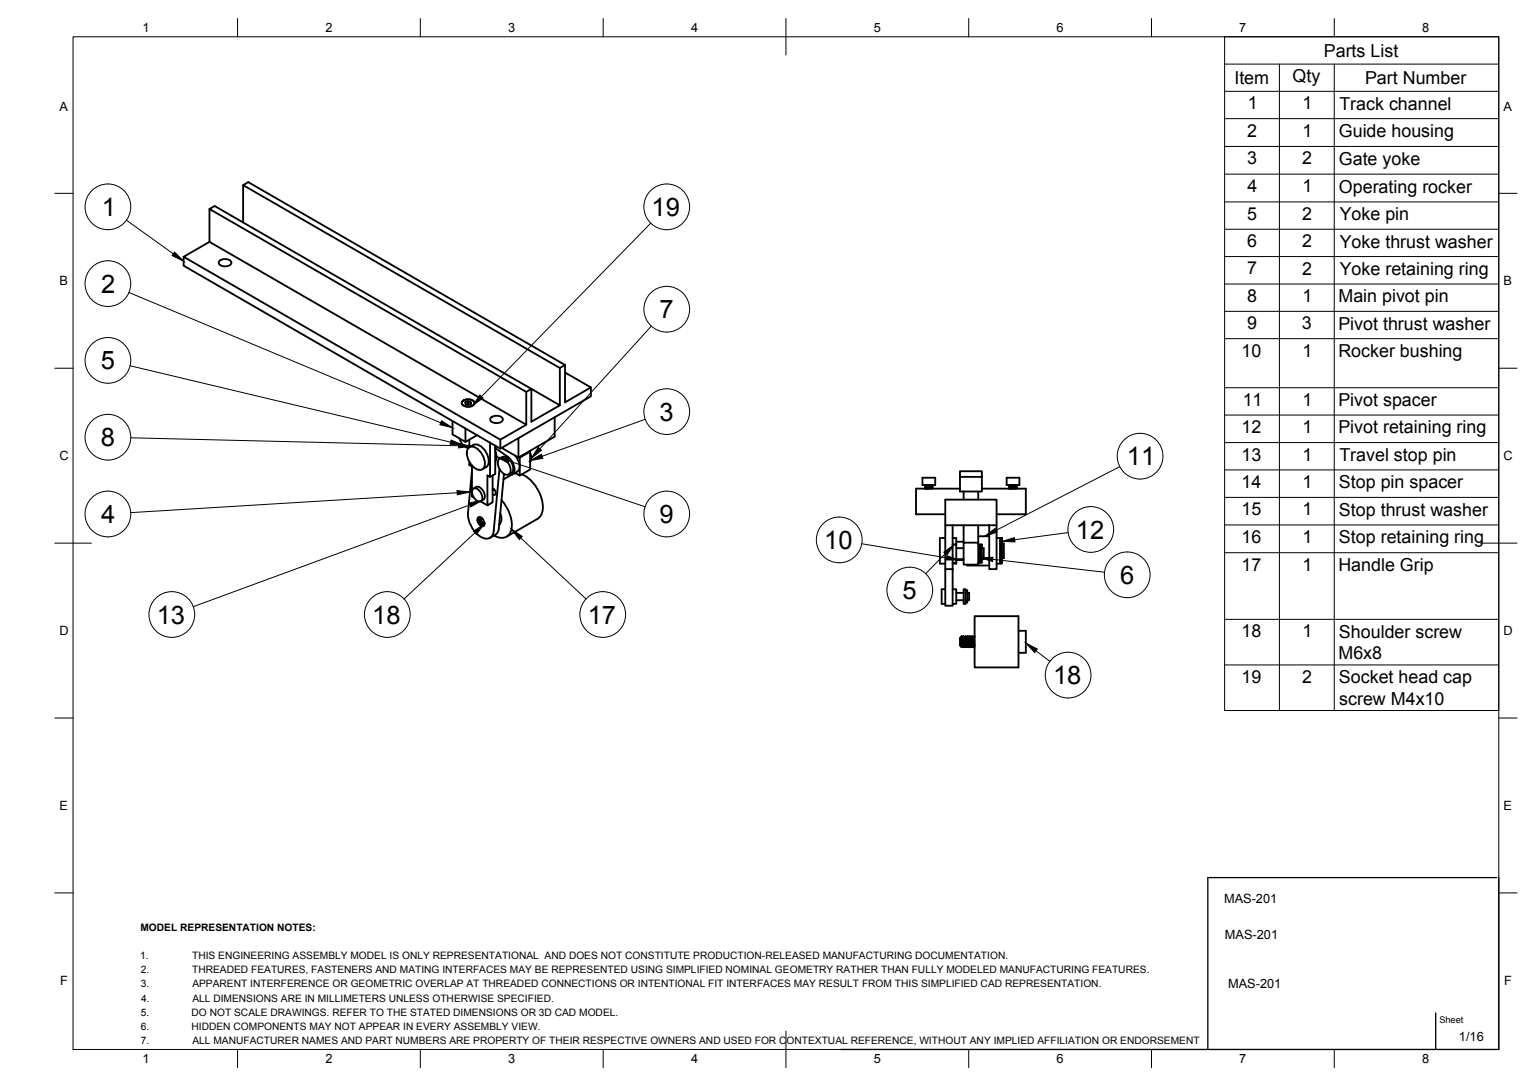
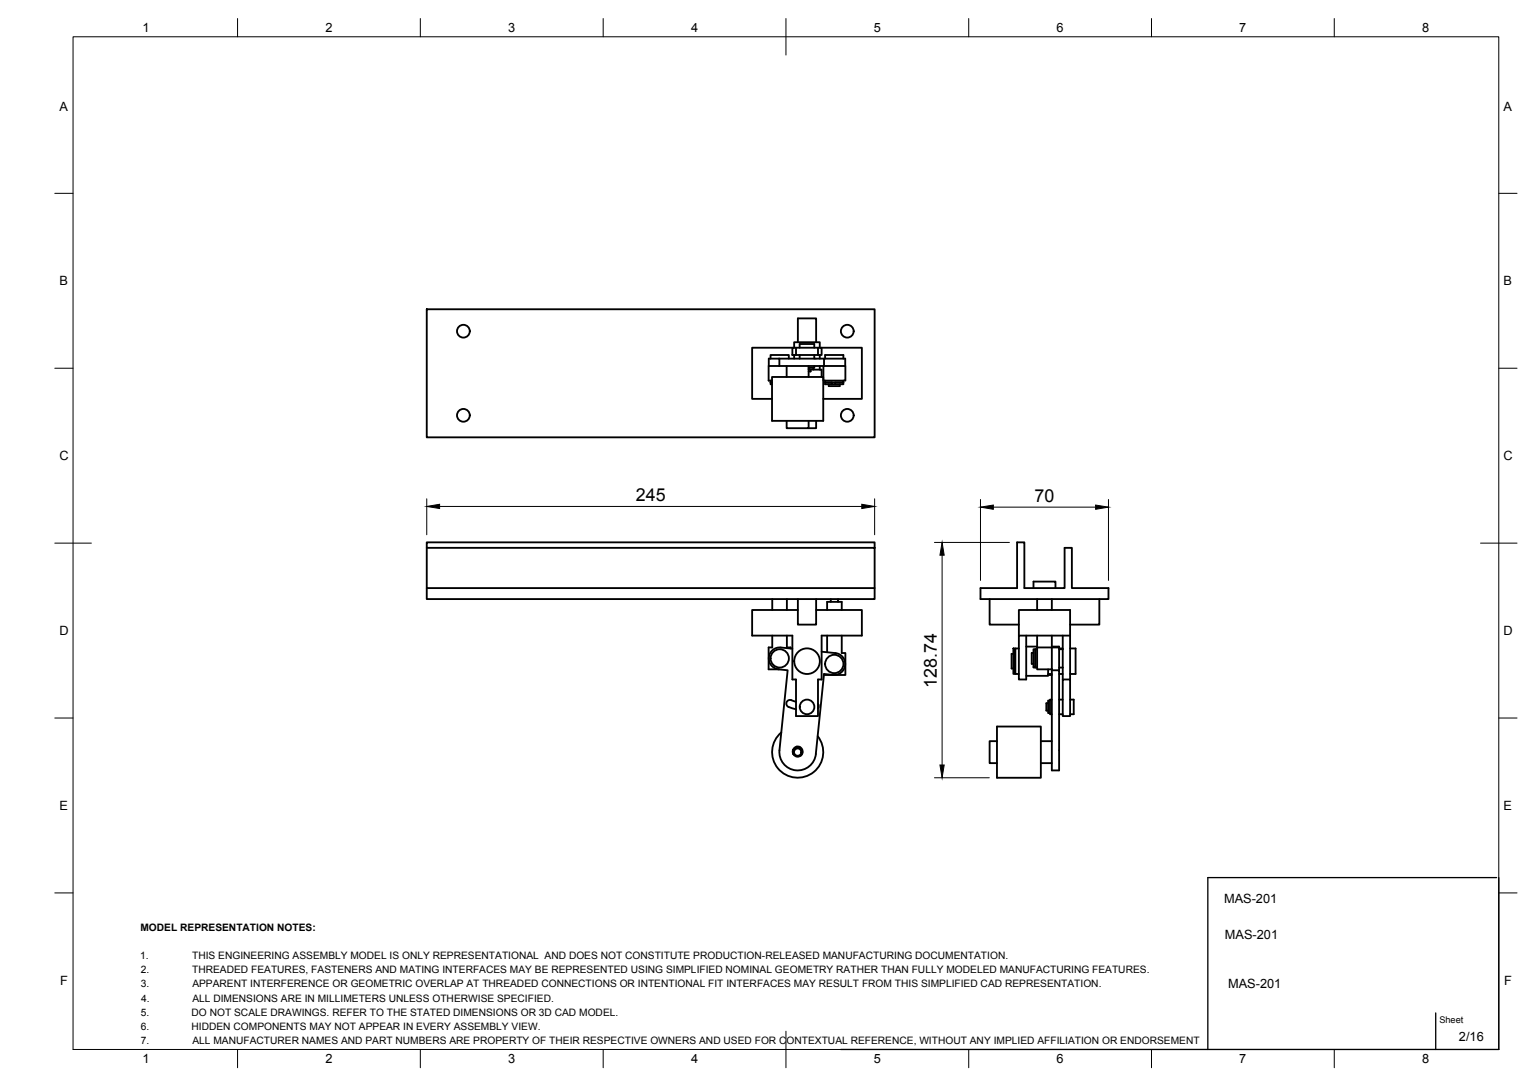
ISO-10303-21;
HEADER;
/* Generated by software containing ST-Developer
 * from STEP Tools, Inc. (www.steptools.com) 
 */

FILE_DESCRIPTION(
/* description */ ('Independent manual two-gate roller-track escapement for nominal30mm d
iameter20mm wide feed rollers. Opposed gates are driven by native capt
ured pin-slot loops with positive curved-slot travel stops at\X\B116de
g. Repeated gate/pin/washer/clip instances, adapted native common bear
ing families, full retaining lips and rotating polymer grip. External 
workpieces, gravity feeder/incline and mount anchors outside assembly.
 No powered-feed compatibility, impact, capacity, safety, force, wear 
or life rating.'),
/* implementation_level */ '2;1');

FILE_NAME(
/* name */ 'MAS-201.step',
/* time_stamp */ '2026-11-08T18:43:23-08:00',
/* author */ (''),
/* organization */ (''),
/* preprocessor_version */ 'ST-DEVELOPER v20.2',
/* originating_system */ 'Autodesk Translation Framework v15.17.0.0',
/* authorisation */ '');

FILE_SCHEMA (('AUTOMOTIVE_DESIGN { 1 0 10303 214 3 1 1 }'));
ENDSEC;

DATA;
#10=MECHANICAL_DESIGN_GEOMETRIC_PRESENTATION_REPRESENTATION('',(#455,#456,
#457,#458,#459,#460,#461,#462,#463,#464,#465,#466,#467,#468,#469,#470,#471,
#472,#473),#19863);
#11=ITEM_DEFINED_TRANSFORMATION($,$,#6654,#7165);
#12=ITEM_DEFINED_TRANSFORMATION($,$,#6703,#7166);
#13=ITEM_DEFINED_TRANSFORMATION($,$,#6899,#7167);
#14=ITEM_DEFINED_TRANSFORMATION($,$,#6827,#7168);
#15=ITEM_DEFINED_TRANSFORMATION($,$,#6926,#7169);
#16=ITEM_DEFINED_TRANSFORMATION($,$,#6962,#7170);
#17=ITEM_DEFINED_TRANSFORMATION($,$,#6899,#7171);
#18=ITEM_DEFINED_TRANSFORMATION($,$,#6926,#7172);
#19=ITEM_DEFINED_TRANSFORMATION($,$,#6971,#7173);
#20=ITEM_DEFINED_TRANSFORMATION($,$,#6944,#7174);
#21=ITEM_DEFINED_TRANSFORMATION($,$,#6991,#7175);
#22=ITEM_DEFINED_TRANSFORMATION($,$,#6962,#7176);
#23=ITEM_DEFINED_TRANSFORMATION($,$,#6971,#7177);
#24=ITEM_DEFINED_TRANSFORMATION($,$,#6982,#7178);
#25=ITEM_DEFINED_TRANSFORMATION($,$,#6991,#7179);
#26=ITEM_DEFINED_TRANSFORMATION($,$,#6991,#7180);
#27=ITEM_DEFINED_TRANSFORMATION($,$,#7000,#7181);
#28=ITEM_DEFINED_TRANSFORMATION($,$,#7009,#7182);
#29=ITEM_DEFINED_TRANSFORMATION($,$,#7020,#7183);
#30=ITEM_DEFINED_TRANSFORMATION($,$,#7038,#7184);
#31=ITEM_DEFINED_TRANSFORMATION($,$,#7047,#7185);
#32=ITEM_DEFINED_TRANSFORMATION($,$,#7056,#7186);
#33=ITEM_DEFINED_TRANSFORMATION($,$,#7067,#7187);
#34=ITEM_DEFINED_TRANSFORMATION($,$,#7076,#7188);
#35=ITEM_DEFINED_TRANSFORMATION($,$,#7117,#7189);
#36=ITEM_DEFINED_TRANSFORMATION($,$,#7117,#7190);
#37=(
REPRESENTATION_RELATIONSHIP($,$,#19935,#19934)
REPRESENTATION_RELATIONSHIP_WITH_TRANSFORMATION(#11)
SHAPE_REPRESENTATION_RELATIONSHIP()
);
#38=(
REPRESENTATION_RELATIONSHIP($,$,#19936,#19934)
REPRESENTATION_RELATIONSHIP_WITH_TRANSFORMATION(#12)
SHAPE_REPRESENTATION_RELATIONSHIP()
);
#39=(
REPRESENTATION_RELATIONSHIP($,$,#19938,#19934)
REPRESENTATION_RELATIONSHIP_WITH_TRANSFORMATION(#13)
SHAPE_REPRESENTATION_RELATIONSHIP()
);
#40=(
REPRESENTATION_RELATIONSHIP($,$,#19937,#19934)
REPRESENTATION_RELATIONSHIP_WITH_TRANSFORMATION(#14)
SHAPE_REPRESENTATION_RELATIONSHIP()
);
#41=(
REPRESENTATION_RELATIONSHIP($,$,#19939,#19934)
REPRESENTATION_RELATIONSHIP_WITH_TRANSFORMATION(#15)
SHAPE_REPRESENTATION_RELATIONSHIP()
);
#42=(
REPRESENTATION_RELATIONSHIP($,$,#19941,#19934)
REPRESENTATION_RELATIONSHIP_WITH_TRANSFORMATION(#16)
SHAPE_REPRESENTATION_RELATIONSHIP()
);
#43=(
REPRESENTATION_RELATIONSHIP($,$,#19938,#19934)
REPRESENTATION_RELATIONSHIP_WITH_TRANSFORMATION(#17)
SHAPE_REPRESENTATION_RELATIONSHIP()
);
#44=(
REPRESENTATION_RELATIONSHIP($,$,#19939,#19934)
REPRESENTATION_RELATIONSHIP_WITH_TRANSFORMATION(#18)
SHAPE_REPRESENTATION_RELATIONSHIP()
);
#45=(
REPRESENTATION_RELATIONSHIP($,$,#19942,#19934)
REPRESENTATION_RELATIONSHIP_WITH_TRANSFORMATION(#19)
SHAPE_REPRESENTATION_RELATIONSHIP()
);
#46=(
REPRESENTATION_RELATIONSHIP($,$,#19940,#19934)
REPRESENTATION_RELATIONSHIP_WITH_TRANSFORMATION(#20)
SHAPE_REPRESENTATION_RELATIONSHIP()
);
#47=(
REPRESENTATION_RELATIONSHIP($,$,#19944,#19934)
REPRESENTATION_RELATIONSHIP_WITH_TRANSFORMATION(#21)
SHAPE_REPRESENTATION_RELATIONSHIP()
);
#48=(
REPRESENTATION_RELATIONSHIP($,$,#19941,#19934)
REPRESENTATION_RELATIONSHIP_WITH_TRANSFORMATION(#22)
SHAPE_REPRESENTATION_RELATIONSHIP()
);
#49=(
REPRESENTATION_RELATIONSHIP($,$,#19942,#19934)
REPRESENTATION_RELATIONSHIP_WITH_TRANSFORMATION(#23)
SHAPE_REPRESENTATION_RELATIONSHIP()
);
#50=(
REPRESENTATION_RELATIONSHIP($,$,#19943,#19934)
REPRESENTATION_RELATIONSHIP_WITH_TRANSFORMATION(#24)
SHAPE_REPRESENTATION_RELATIONSHIP()
);
#51=(
REPRESENTATION_RELATIONSHIP($,$,#19944,#19934)
REPRESENTATION_RELATIONSHIP_WITH_TRANSFORMATION(#25)
SHAPE_REPRESENTATION_RELATIONSHIP()
);
#52=(
REPRESENTATION_RELATIONSHIP($,$,#19944,#19934)
REPRESENTATION_RELATIONSHIP_WITH_TRANSFORMATION(#26)
SHAPE_REPRESENTATION_RELATIONSHIP()
);
#53=(
REPRESENTATION_RELATIONSHIP($,$,#19945,#19934)
REPRESENTATION_RELATIONSHIP_WITH_TRANSFORMATION(#27)
SHAPE_REPRESENTATION_RELATIONSHIP()
);
#54=(
REPRESENTATION_RELATIONSHIP($,$,#19946,#19934)
REPRESENTATION_RELATIONSHIP_WITH_TRANSFORMATION(#28)
SHAPE_REPRESENTATION_RELATIONSHIP()
);
#55=(
REPRESENTATION_RELATIONSHIP($,$,#19947,#19934)
REPRESENTATION_RELATIONSHIP_WITH_TRANSFORMATION(#29)
SHAPE_REPRESENTATION_RELATIONSHIP()
);
#56=(
REPRESENTATION_RELATIONSHIP($,$,#19948,#19934)
REPRESENTATION_RELATIONSHIP_WITH_TRANSFORMATION(#30)
SHAPE_REPRESENTATION_RELATIONSHIP()
);
#57=(
REPRESENTATION_RELATIONSHIP($,$,#19949,#19934)
REPRESENTATION_RELATIONSHIP_WITH_TRANSFORMATION(#31)
SHAPE_REPRESENTATION_RELATIONSHIP()
);
#58=(
REPRESENTATION_RELATIONSHIP($,$,#19950,#19934)
REPRESENTATION_RELATIONSHIP_WITH_TRANSFORMATION(#32)
SHAPE_REPRESENTATION_RELATIONSHIP()
);
#59=(
REPRESENTATION_RELATIONSHIP($,$,#19951,#19934)
REPRESENTATION_RELATIONSHIP_WITH_TRANSFORMATION(#33)
SHAPE_REPRESENTATION_RELATIONSHIP()
);
#60=(
REPRESENTATION_RELATIONSHIP($,$,#19952,#19934)
REPRESENTATION_RELATIONSHIP_WITH_TRANSFORMATION(#34)
SHAPE_REPRESENTATION_RELATIONSHIP()
);
#61=(
REPRESENTATION_RELATIONSHIP($,$,#19953,#19934)
REPRESENTATION_RELATIONSHIP_WITH_TRANSFORMATION(#35)
SHAPE_REPRESENTATION_RELATIONSHIP()
);
#62=(
REPRESENTATION_RELATIONSHIP($,$,#19953,#19934)
REPRESENTATION_RELATIONSHIP_WITH_TRANSFORMATION(#36)
SHAPE_REPRESENTATION_RELATIONSHIP()
);
#63=CONTEXT_DEPENDENT_SHAPE_REPRESENTATION(#37,#19908);
#64=CONTEXT_DEPENDENT_SHAPE_REPRESENTATION(#38,#19909);
#65=CONTEXT_DEPENDENT_SHAPE_REPRESENTATION(#39,#19910);
#66=CONTEXT_DEPENDENT_SHAPE_REPRESENTATION(#40,#19911);
#67=CONTEXT_DEPENDENT_SHAPE_REPRESENTATION(#41,#19912);
#68=CONTEXT_DEPENDENT_SHAPE_REPRESENTATION(#42,#19913);
#69=CONTEXT_DEPENDENT_SHAPE_REPRESENTATION(#43,#19914);
#70=CONTEXT_DEPENDENT_SHAPE_REPRESENTATION(#44,#19915);
#71=CONTEXT_DEPENDENT_SHAPE_REPRESENTATION(#45,#19916);
#72=CONTEXT_DEPENDENT_SHAPE_REPRESENTATION(#46,#19917);
#73=CONTEXT_DEPENDENT_SHAPE_REPRESENTATION(#47,#19918);
#74=CONTEXT_DEPENDENT_SHAPE_REPRESENTATION(#48,#19919);
#75=CONTEXT_DEPENDENT_SHAPE_REPRESENTATION(#49,#19920);
#76=CONTEXT_DEPENDENT_SHAPE_REPRESENTATION(#50,#19921);
#77=CONTEXT_DEPENDENT_SHAPE_REPRESENTATION(#51,#19922);
#78=CONTEXT_DEPENDENT_SHAPE_REPRESENTATION(#52,#19923);
#79=CONTEXT_DEPENDENT_SHAPE_REPRESENTATION(#53,#19924);
#80=CONTEXT_DEPENDENT_SHAPE_REPRESENTATION(#54,#19925);
#81=CONTEXT_DEPENDENT_SHAPE_REPRESENTATION(#55,#19926);
#82=CONTEXT_DEPENDENT_SHAPE_REPRESENTATION(#56,#19927);
#83=CONTEXT_DEPENDENT_SHAPE_REPRESENTATION(#57,#19928);
#84=CONTEXT_DEPENDENT_SHAPE_REPRESENTATION(#58,#19929);
#85=CONTEXT_DEPENDENT_SHAPE_REPRESENTATION(#59,#19930);
#86=CONTEXT_DEPENDENT_SHAPE_REPRESENTATION(#60,#19931);
#87=CONTEXT_DEPENDENT_SHAPE_REPRESENTATION(#61,#19932);
#88=CONTEXT_DEPENDENT_SHAPE_REPRESENTATION(#62,#19933);
#89=NEXT_ASSEMBLY_USAGE_OCCURRENCE('Track channel:1','Track channel:1',
'Track channel:1',#19955,#19956,'Track channel:1');
#90=NEXT_ASSEMBLY_USAGE_OCCURRENCE('Guide housing:1','Guide housing:1',
'Guide housing:1',#19955,#19957,'Guide housing:1');
#91=NEXT_ASSEMBLY_USAGE_OCCURRENCE('Gate yoke:1','Gate yoke:1',
'Gate yoke:1',#19955,#19959,'Gate yoke:1');
#92=NEXT_ASSEMBLY_USAGE_OCCURRENCE('Operating rocker:1',
'Operating rocker:1','Operating rocker:1',#19955,#19958,
'Operating rocker:1');
#93=NEXT_ASSEMBLY_USAGE_OCCURRENCE('Yoke pin:1','Yoke pin:1',
'Yoke pin:1',#19955,#19960,'Yoke pin:1');
#94=NEXT_ASSEMBLY_USAGE_OCCURRENCE('Yoke thrust washer:1',
'Yoke thrust washer:1','Yoke thrust washer:1',#19955,#19962,
'Yoke thrust washer:1');
#95=NEXT_ASSEMBLY_USAGE_OCCURRENCE('Gate yoke:2','Gate yoke:2',
'Gate yoke:2',#19955,#19959,'Gate yoke:2');
#96=NEXT_ASSEMBLY_USAGE_OCCURRENCE('Yoke pin:2','Yoke pin:2',
'Yoke pin:2',#19955,#19960,'Yoke pin:2');
#97=NEXT_ASSEMBLY_USAGE_OCCURRENCE('Yoke retaining ring:1',
'Yoke retaining ring:1','Yoke retaining ring:1',#19955,#19963,
'Yoke retaining ring:1');
#98=NEXT_ASSEMBLY_USAGE_OCCURRENCE('Main pivot pin:1',
'Main pivot pin:1','Main pivot pin:1',#19955,#19961,'Main pivot pin:1');
#99=NEXT_ASSEMBLY_USAGE_OCCURRENCE('Pivot thrust washer:1',
'Pivot thrust washer:1','Pivot thrust washer:1',#19955,#19965,
'Pivot thrust washer:1');
#100=NEXT_ASSEMBLY_USAGE_OCCURRENCE('Yoke thrust washer:2',
'Yoke thrust washer:2','Yoke thrust washer:2',#19955,#19962,
'Yoke thrust washer:2');
#101=NEXT_ASSEMBLY_USAGE_OCCURRENCE('Yoke retaining ring:2',
'Yoke retaining ring:2','Yoke retaining ring:2',#19955,#19963,
'Yoke retaining ring:2');
#102=NEXT_ASSEMBLY_USAGE_OCCURRENCE('Rocker bushing:1',
'Rocker bushing:1','Rocker bushing:1',#19955,#19964,'Rocker bushing:1');
#103=NEXT_ASSEMBLY_USAGE_OCCURRENCE('Pivot thrust washer:2',
'Pivot thrust washer:2','Pivot thrust washer:2',#19955,#19965,
'Pivot thrust washer:2');
#104=NEXT_ASSEMBLY_USAGE_OCCURRENCE('Pivot thrust washer:3',
'Pivot thrust washer:3','Pivot thrust washer:3',#19955,#19965,
'Pivot thrust washer:3');
#105=NEXT_ASSEMBLY_USAGE_OCCURRENCE('Pivot spacer:1','Pivot spacer:1',
'Pivot spacer:1',#19955,#19966,'Pivot spacer:1');
#106=NEXT_ASSEMBLY_USAGE_OCCURRENCE('Pivot retaining ring:1',
'Pivot retaining ring:1','Pivot retaining ring:1',#19955,#19967,
'Pivot retaining ring:1');
#107=NEXT_ASSEMBLY_USAGE_OCCURRENCE('Travel stop pin:1',
'Travel stop pin:1','Travel stop pin:1',#19955,#19968,
'Travel stop pin:1');
#108=NEXT_ASSEMBLY_USAGE_OCCURRENCE('Stop pin spacer:1',
'Stop pin spacer:1','Stop pin spacer:1',#19955,#19969,
'Stop pin spacer:1');
#109=NEXT_ASSEMBLY_USAGE_OCCURRENCE('Stop thrust washer:1',
'Stop thrust washer:1','Stop thrust washer:1',#19955,#19970,
'Stop thrust washer:1');
#110=NEXT_ASSEMBLY_USAGE_OCCURRENCE('Stop retaining ring:1',
'Stop retaining ring:1','Stop retaining ring:1',#19955,#19971,
'Stop retaining ring:1');
#111=NEXT_ASSEMBLY_USAGE_OCCURRENCE('Handle grip:1','Handle grip:1',
'Handle grip:1',#19955,#19972,'Handle grip:1');
#112=NEXT_ASSEMBLY_USAGE_OCCURRENCE('Shoulder screw M6x8:1',
'Shoulder screw M6x8:1','Shoulder screw M6x8:1',#19955,#19973,
'Shoulder screw M6x8:1');
#113=NEXT_ASSEMBLY_USAGE_OCCURRENCE('Socket head cap screw M4x10:1',
'Socket head cap screw M4x10:1','Socket head cap screw M4x10:1',#19955,
#19974,'Socket head cap screw M4x10:1');
#114=NEXT_ASSEMBLY_USAGE_OCCURRENCE('Socket head cap screw M4x10:2',
'Socket head cap screw M4x10:2','Socket head cap screw M4x10:2',#19955,
#19974,'Socket head cap screw M4x10:2');
#115=CONICAL_SURFACE('',#7094,2.5,0.785398163397448);
#116=CONICAL_SURFACE('',#7146,1.5,0.785398163397449);
#117=B_SPLINE_SURFACE_WITH_KNOTS('',3,3,((#11345,#11346,#11347,#11348,#11349,
#11350,#11351,#11352,#11353,#11354,#11355,#11356,#11357,#11358,#11359,#11360,
#11361,#11362,#11363,#11364,#11365,#11366,#11367,#11368,#11369,#11370,#11371,
#11372,#11373,#11374,#11375,#11376,#11377,#11378,#11379,#11380,#11381,#11382,
#11383,#11384,#11385,#11386,#11387,#11388,#11389,#11390,#11391,#11392,#11393,
#11394,#11395,#11396,#11397,#11398,#11399,#11400,#11401,#11402,#11403,#11404,
#11405,#11406,#11407,#11408,#11409,#11410,#11411,#11412,#11413,#11414,#11415,
#11416,#11417,#11418,#11419,#11420,#11421,#11422,#11423,#11424,#11425,#11426,
#11427,#11428,#11429,#11430,#11431,#11432,#11433,#11434,#11435,#11436,#11437,
#11438,#11439,#11440,#11441,#11442,#11443,#11444,#11445,#11446,#11447,#11448),
(#11449,#11450,#11451,#11452,#11453,#11454,#11455,#11456,#11457,#11458,
#11459,#11460,#11461,#11462,#11463,#11464,#11465,#11466,#11467,#11468,#11469,
#11470,#11471,#11472,#11473,#11474,#11475,#11476,#11477,#11478,#11479,#11480,
#11481,#11482,#11483,#11484,#11485,#11486,#11487,#11488,#11489,#11490,#11491,
#11492,#11493,#11494,#11495,#11496,#11497,#11498,#11499,#11500,#11501,#11502,
#11503,#11504,#11505,#11506,#11507,#11508,#11509,#11510,#11511,#11512,#11513,
#11514,#11515,#11516,#11517,#11518,#11519,#11520,#11521,#11522,#11523,#11524,
#11525,#11526,#11527,#11528,#11529,#11530,#11531,#11532,#11533,#11534,#11535,
#11536,#11537,#11538,#11539,#11540,#11541,#11542,#11543,#11544,#11545,#11546,
#11547,#11548,#11549,#11550,#11551,#11552),(#11553,#11554,#11555,#11556,
#11557,#11558,#11559,#11560,#11561,#11562,#11563,#11564,#11565,#11566,#11567,
#11568,#11569,#11570,#11571,#11572,#11573,#11574,#11575,#11576,#11577,#11578,
#11579,#11580,#11581,#11582,#11583,#11584,#11585,#11586,#11587,#11588,#11589,
#11590,#11591,#11592,#11593,#11594,#11595,#11596,#11597,#11598,#11599,#11600,
#11601,#11602,#11603,#11604,#11605,#11606,#11607,#11608,#11609,#11610,#11611,
#11612,#11613,#11614,#11615,#11616,#11617,#11618,#11619,#11620,#11621,#11622,
#11623,#11624,#11625,#11626,#11627,#11628,#11629,#11630,#11631,#11632,#11633,
#11634,#11635,#11636,#11637,#11638,#11639,#11640,#11641,#11642,#11643,#11644,
#11645,#11646,#11647,#11648,#11649,#11650,#11651,#11652,#11653,#11654,#11655,
#11656),(#11657,#11658,#11659,#11660,#11661,#11662,#11663,#11664,#11665,
#11666,#11667,#11668,#11669,#11670,#11671,#11672,#11673,#11674,#11675,#11676,
#11677,#11678,#11679,#11680,#11681,#11682,#11683,#11684,#11685,#11686,#11687,
#11688,#11689,#11690,#11691,#11692,#11693,#11694,#11695,#11696,#11697,#11698,
#11699,#11700,#11701,#11702,#11703,#11704,#11705,#11706,#11707,#11708,#11709,
#11710,#11711,#11712,#11713,#11714,#11715,#11716,#11717,#11718,#11719,#11720,
#11721,#11722,#11723,#11724,#11725,#11726,#11727,#11728,#11729,#11730,#11731,
#11732,#11733,#11734,#11735,#11736,#11737,#11738,#11739,#11740,#11741,#11742,
#11743,#11744,#11745,#11746,#11747,#11748,#11749,#11750,#11751,#11752,#11753,
#11754,#11755,#11756,#11757,#11758,#11759,#11760)),.UNSPECIFIED.,.F.,.F.,
 .F.,(4,4),(4,1,1,1,1,1,1,1,1,1,1,1,1,1,1,1,1,1,1,1,1,1,1,1,1,1,1,1,1,1,
1,1,1,1,1,1,1,1,1,1,1,1,1,1,1,1,1,1,1,1,1,1,1,1,1,1,1,1,1,1,1,1,1,1,1,1,
1,1,1,1,1,1,1,1,1,1,1,1,1,1,1,1,1,1,1,1,1,1,1,1,1,1,1,1,1,1,1,1,1,1,1,4),
(0.,0.0448889834294942),(11.8615800042566,12.8591085386932,13.8566370731298,
14.8541656075664,15.851694142003,16.8492226764396,17.8467512108762,18.8442797453128,
19.8418082797494,20.839336814186,21.8368653486226,22.8343938830592,23.8319224174958,
24.8294509519324,25.826979486369,26.8245080208056,27.8220365552422,28.8195650896788,
29.8170936241154,30.814622158552,31.8121506929886,32.8096792274252,33.8072077618618,
34.8047362962984,35.802264830735,36.7997933651716,37.7973218996082,38.7948504340448,
39.7923789684814,40.789907502918,41.7874360373546,42.7849645717912,43.7824931062278,
44.7800216406644,45.777550175101,46.7750787095376,47.7726072439742,48.7701357784108,
49.7676643128474,50.765192847284,51.7627213817206,52.7602499161572,53.7577784505938,
54.7553069850304,55.752835519467,56.7503640539036,57.7478925883402,58.7454211227768,
59.7429496572134,60.74047819165,61.7380067260866,62.7355352605232,63.7330637949598,
64.7305923293964,65.728120863833,66.7256493982696,67.7231779327062,68.7207064671428,
69.7182350015794,70.715763536016,71.7132920704526,72.7108206048892,73.7083491393258,
74.7058776737624,75.703406208199,76.7009347426356,77.6984632770722,78.6959918115088,
79.6935203459454,80.691048880382,81.6885774148186,82.6861059492552,83.6836344836918,
84.6811630181284,85.678691552565,86.6762200870016,87.6737486214382,88.6712771558748,
89.6688056903114,90.666334224748,91.6638627591846,92.6613912936212,93.6589198280578,
94.6564483624944,95.653976896931,96.6515054313676,97.6490339658042,98.6465625002408,
99.6440910346774,100.641619569114,101.639148103551,102.636676637987,103.634205172424,
104.63173370686,105.629262241297,106.626790775734,107.62431931017,108.621847844607,
109.619376379043,110.61690491348,111.614433447917,112.611961982353),
 .UNSPECIFIED.);
#118=B_SPLINE_SURFACE_WITH_KNOTS('',3,3,((#11868,#11869,#11870,#11871,#11872,
#11873,#11874,#11875,#11876,#11877,#11878,#11879,#11880,#11881,#11882,#11883,
#11884,#11885,#11886,#11887,#11888,#11889,#11890,#11891,#11892,#11893,#11894,
#11895,#11896,#11897,#11898,#11899,#11900,#11901,#11902,#11903,#11904,#11905,
#11906,#11907,#11908,#11909,#11910,#11911,#11912,#11913,#11914,#11915,#11916,
#11917,#11918,#11919,#11920,#11921,#11922,#11923,#11924,#11925,#11926,#11927,
#11928,#11929,#11930,#11931,#11932,#11933,#11934,#11935,#11936,#11937,#11938,
#11939,#11940,#11941,#11942,#11943,#11944,#11945,#11946,#11947,#11948,#11949,
#11950,#11951,#11952,#11953,#11954,#11955,#11956,#11957,#11958,#11959,#11960,
#11961,#11962,#11963,#11964,#11965,#11966,#11967,#11968,#11969,#11970,#11971),
(#11972,#11973,#11974,#11975,#11976,#11977,#11978,#11979,#11980,#11981,
#11982,#11983,#11984,#11985,#11986,#11987,#11988,#11989,#11990,#11991,#11992,
#11993,#11994,#11995,#11996,#11997,#11998,#11999,#12000,#12001,#12002,#12003,
#12004,#12005,#12006,#12007,#12008,#12009,#12010,#12011,#12012,#12013,#12014,
#12015,#12016,#12017,#12018,#12019,#12020,#12021,#12022,#12023,#12024,#12025,
#12026,#12027,#12028,#12029,#12030,#12031,#12032,#12033,#12034,#12035,#12036,
#12037,#12038,#12039,#12040,#12041,#12042,#12043,#12044,#12045,#12046,#12047,
#12048,#12049,#12050,#12051,#12052,#12053,#12054,#12055,#12056,#12057,#12058,
#12059,#12060,#12061,#12062,#12063,#12064,#12065,#12066,#12067,#12068,#12069,
#12070,#12071,#12072,#12073,#12074,#12075),(#12076,#12077,#12078,#12079,
#12080,#12081,#12082,#12083,#12084,#12085,#12086,#12087,#12088,#12089,#12090,
#12091,#12092,#12093,#12094,#12095,#12096,#12097,#12098,#12099,#12100,#12101,
#12102,#12103,#12104,#12105,#12106,#12107,#12108,#12109,#12110,#12111,#12112,
#12113,#12114,#12115,#12116,#12117,#12118,#12119,#12120,#12121,#12122,#12123,
#12124,#12125,#12126,#12127,#12128,#12129,#12130,#12131,#12132,#12133,#12134,
#12135,#12136,#12137,#12138,#12139,#12140,#12141,#12142,#12143,#12144,#12145,
#12146,#12147,#12148,#12149,#12150,#12151,#12152,#12153,#12154,#12155,#12156,
#12157,#12158,#12159,#12160,#12161,#12162,#12163,#12164,#12165,#12166,#12167,
#12168,#12169,#12170,#12171,#12172,#12173,#12174,#12175,#12176,#12177,#12178,
#12179),(#12180,#12181,#12182,#12183,#12184,#12185,#12186,#12187,#12188,
#12189,#12190,#12191,#12192,#12193,#12194,#12195,#12196,#12197,#12198,#12199,
#12200,#12201,#12202,#12203,#12204,#12205,#12206,#12207,#12208,#12209,#12210,
#12211,#12212,#12213,#12214,#12215,#12216,#12217,#12218,#12219,#12220,#12221,
#12222,#12223,#12224,#12225,#12226,#12227,#12228,#12229,#12230,#12231,#12232,
#12233,#12234,#12235,#12236,#12237,#12238,#12239,#12240,#12241,#12242,#12243,
#12244,#12245,#12246,#12247,#12248,#12249,#12250,#12251,#12252,#12253,#12254,
#12255,#12256,#12257,#12258,#12259,#12260,#12261,#12262,#12263,#12264,#12265,
#12266,#12267,#12268,#12269,#12270,#12271,#12272,#12273,#12274,#12275,#12276,
#12277,#12278,#12279,#12280,#12281,#12282,#12283)),.UNSPECIFIED.,.F.,.F.,
 .F.,(4,4),(4,1,1,1,1,1,1,1,1,1,1,1,1,1,1,1,1,1,1,1,1,1,1,1,1,1,1,1,1,1,
1,1,1,1,1,1,1,1,1,1,1,1,1,1,1,1,1,1,1,1,1,1,1,1,1,1,1,1,1,1,1,1,1,1,1,1,
1,1,1,1,1,1,1,1,1,1,1,1,1,1,1,1,1,1,1,1,1,1,1,1,1,1,1,1,1,1,1,1,1,1,1,4),
(0.,0.0448889834294942),(14.3981410127769,15.3956695472135,16.3931980816501,
17.3907266160867,18.3882551505233,19.3857836849599,20.3833122193965,21.3808407538331,
22.3783692882697,23.3758978227063,24.3734263571429,25.3709548915795,26.3684834260161,
27.3660119604527,28.3635404948893,29.3610690293259,30.3585975637625,31.3561260981991,
32.3536546326357,33.3511831670723,34.3487117015089,35.3462402359455,36.3437687703821,
37.3412973048187,38.3388258392553,39.3363543736919,40.3338829081285,41.3314114425651,
42.3289399770017,43.3264685114383,44.3239970458749,45.3215255803115,46.3190541147481,
47.3165826491847,48.3141111836213,49.3116397180579,50.3091682524945,51.3066967869311,
52.3042253213677,53.3017538558043,54.2992823902409,55.2968109246775,56.294339459114,
57.2918679935507,58.2893965279873,59.2869250624238,60.2844535968605,61.281982131297,
62.2795106657336,63.2770392001703,64.2745677346068,65.2720962690434,66.26962480348,
67.2671533379167,68.2646818723532,69.2622104067898,70.2597389412264,71.257267475663,
72.2547960100996,73.2523245445362,74.2498530789728,75.2473816134094,76.244910147846,
77.2424386822826,78.2399672167192,79.2374957511558,80.2350242855924,81.232552820029,
82.2300813544656,83.2276098889022,84.2251384233388,85.2226669577754,86.220195492212,
87.2177240266486,88.2152525610852,89.2127810955218,90.2103096299584,91.207838164395,
92.2053666988316,93.2028952332682,94.2004237677048,95.1979523021414,96.195480836578,
97.1930093710146,98.1905379054512,99.1880664398878,100.185594974324,101.183123508761,
102.180652043198,103.178180577634,104.175709112071,105.173237646507,106.170766180944,
107.168294715381,108.165823249817,109.163351784254,110.16088031869,111.158408853127,
112.155937387564,113.153465922,114.150994456437,115.148522990873),
 .UNSPECIFIED.);
#119=B_SPLINE_SURFACE_WITH_KNOTS('',3,3,((#12588,#12589,#12590,#12591,#12592,
#12593,#12594,#12595,#12596,#12597,#12598,#12599,#12600,#12601,#12602,#12603,
#12604,#12605,#12606,#12607,#12608,#12609,#12610,#12611,#12612,#12613,#12614,
#12615,#12616,#12617,#12618,#12619,#12620,#12621,#12622,#12623,#12624,#12625,
#12626,#12627,#12628,#12629,#12630,#12631,#12632,#12633,#12634,#12635,#12636,
#12637,#12638,#12639,#12640,#12641,#12642,#12643,#12644,#12645,#12646,#12647,
#12648,#12649,#12650,#12651,#12652,#12653,#12654,#12655,#12656,#12657,#12658,
#12659,#12660,#12661,#12662,#12663,#12664,#12665,#12666,#12667,#12668,#12669,
#12670,#12671,#12672,#12673,#12674,#12675,#12676,#12677,#12678,#12679,#12680,
#12681,#12682,#12683,#12684,#12685,#12686,#12687,#12688,#12689,#12690,#12691),
(#12692,#12693,#12694,#12695,#12696,#12697,#12698,#12699,#12700,#12701,
#12702,#12703,#12704,#12705,#12706,#12707,#12708,#12709,#12710,#12711,#12712,
#12713,#12714,#12715,#12716,#12717,#12718,#12719,#12720,#12721,#12722,#12723,
#12724,#12725,#12726,#12727,#12728,#12729,#12730,#12731,#12732,#12733,#12734,
#12735,#12736,#12737,#12738,#12739,#12740,#12741,#12742,#12743,#12744,#12745,
#12746,#12747,#12748,#12749,#12750,#12751,#12752,#12753,#12754,#12755,#12756,
#12757,#12758,#12759,#12760,#12761,#12762,#12763,#12764,#12765,#12766,#12767,
#12768,#12769,#12770,#12771,#12772,#12773,#12774,#12775,#12776,#12777,#12778,
#12779,#12780,#12781,#12782,#12783,#12784,#12785,#12786,#12787,#12788,#12789,
#12790,#12791,#12792,#12793,#12794,#12795),(#12796,#12797,#12798,#12799,
#12800,#12801,#12802,#12803,#12804,#12805,#12806,#12807,#12808,#12809,#12810,
#12811,#12812,#12813,#12814,#12815,#12816,#12817,#12818,#12819,#12820,#12821,
#12822,#12823,#12824,#12825,#12826,#12827,#12828,#12829,#12830,#12831,#12832,
#12833,#12834,#12835,#12836,#12837,#12838,#12839,#12840,#12841,#12842,#12843,
#12844,#12845,#12846,#12847,#12848,#12849,#12850,#12851,#12852,#12853,#12854,
#12855,#12856,#12857,#12858,#12859,#12860,#12861,#12862,#12863,#12864,#12865,
#12866,#12867,#12868,#12869,#12870,#12871,#12872,#12873,#12874,#12875,#12876,
#12877,#12878,#12879,#12880,#12881,#12882,#12883,#12884,#12885,#12886,#12887,
#12888,#12889,#12890,#12891,#12892,#12893,#12894,#12895,#12896,#12897,#12898,
#12899),(#12900,#12901,#12902,#12903,#12904,#12905,#12906,#12907,#12908,
#12909,#12910,#12911,#12912,#12913,#12914,#12915,#12916,#12917,#12918,#12919,
#12920,#12921,#12922,#12923,#12924,#12925,#12926,#12927,#12928,#12929,#12930,
#12931,#12932,#12933,#12934,#12935,#12936,#12937,#12938,#12939,#12940,#12941,
#12942,#12943,#12944,#12945,#12946,#12947,#12948,#12949,#12950,#12951,#12952,
#12953,#12954,#12955,#12956,#12957,#12958,#12959,#12960,#12961,#12962,#12963,
#12964,#12965,#12966,#12967,#12968,#12969,#12970,#12971,#12972,#12973,#12974,
#12975,#12976,#12977,#12978,#12979,#12980,#12981,#12982,#12983,#12984,#12985,
#12986,#12987,#12988,#12989,#12990,#12991,#12992,#12993,#12994,#12995,#12996,
#12997,#12998,#12999,#13000,#13001,#13002,#13003)),.UNSPECIFIED.,.F.,.F.,
 .F.,(4,4),(4,1,1,1,1,1,1,1,1,1,1,1,1,1,1,1,1,1,1,1,1,1,1,1,1,1,1,1,1,1,
1,1,1,1,1,1,1,1,1,1,1,1,1,1,1,1,1,1,1,1,1,1,1,1,1,1,1,1,1,1,1,1,1,1,1,1,
1,1,1,1,1,1,1,1,1,1,1,1,1,1,1,1,1,1,1,1,1,1,1,1,1,1,1,1,1,1,1,1,1,1,1,4),
(0.,0.0448889834294942),(11.8615800042566,12.8591085386932,13.8566370731298,
14.8541656075664,15.851694142003,16.8492226764396,17.8467512108762,18.8442797453128,
19.8418082797494,20.839336814186,21.8368653486226,22.8343938830592,23.8319224174958,
24.8294509519324,25.826979486369,26.8245080208056,27.8220365552422,28.8195650896788,
29.8170936241154,30.814622158552,31.8121506929886,32.8096792274252,33.8072077618618,
34.8047362962984,35.802264830735,36.7997933651716,37.7973218996082,38.7948504340448,
39.7923789684814,40.789907502918,41.7874360373546,42.7849645717912,43.7824931062278,
44.7800216406644,45.777550175101,46.7750787095376,47.7726072439742,48.7701357784108,
49.7676643128474,50.765192847284,51.7627213817206,52.7602499161572,53.7577784505938,
54.7553069850304,55.752835519467,56.7503640539036,57.7478925883402,58.7454211227768,
59.7429496572134,60.74047819165,61.7380067260866,62.7355352605232,63.7330637949598,
64.7305923293964,65.728120863833,66.7256493982696,67.7231779327062,68.7207064671428,
69.7182350015794,70.715763536016,71.7132920704526,72.7108206048892,73.7083491393258,
74.7058776737624,75.703406208199,76.7009347426356,77.6984632770722,78.6959918115088,
79.6935203459454,80.691048880382,81.6885774148186,82.6861059492552,83.6836344836918,
84.6811630181284,85.678691552565,86.6762200870016,87.6737486214382,88.6712771558748,
89.6688056903114,90.666334224748,91.6638627591846,92.6613912936212,93.6589198280578,
94.6564483624944,95.653976896931,96.6515054313676,97.6490339658042,98.6465625002408,
99.6440910346774,100.641619569114,101.639148103551,102.636676637987,103.634205172424,
104.63173370686,105.629262241297,106.626790775734,107.62431931017,108.621847844607,
109.619376379043,110.61690491348,111.614433447917,112.611961982353),
 .UNSPECIFIED.);
#120=B_SPLINE_SURFACE_WITH_KNOTS('',3,3,((#13111,#13112,#13113,#13114,#13115,
#13116,#13117,#13118,#13119,#13120,#13121,#13122,#13123,#13124,#13125,#13126,
#13127,#13128,#13129,#13130,#13131,#13132,#13133,#13134,#13135,#13136,#13137,
#13138,#13139,#13140,#13141,#13142,#13143,#13144,#13145,#13146,#13147,#13148,
#13149,#13150,#13151,#13152,#13153,#13154,#13155,#13156,#13157,#13158,#13159,
#13160,#13161,#13162,#13163,#13164,#13165,#13166,#13167,#13168,#13169,#13170,
#13171,#13172,#13173,#13174,#13175,#13176,#13177,#13178,#13179,#13180,#13181,
#13182,#13183,#13184,#13185,#13186,#13187,#13188,#13189,#13190,#13191,#13192,
#13193,#13194,#13195,#13196,#13197,#13198,#13199,#13200,#13201,#13202,#13203,
#13204,#13205,#13206,#13207,#13208,#13209,#13210,#13211,#13212,#13213,#13214),
(#13215,#13216,#13217,#13218,#13219,#13220,#13221,#13222,#13223,#13224,
#13225,#13226,#13227,#13228,#13229,#13230,#13231,#13232,#13233,#13234,#13235,
#13236,#13237,#13238,#13239,#13240,#13241,#13242,#13243,#13244,#13245,#13246,
#13247,#13248,#13249,#13250,#13251,#13252,#13253,#13254,#13255,#13256,#13257,
#13258,#13259,#13260,#13261,#13262,#13263,#13264,#13265,#13266,#13267,#13268,
#13269,#13270,#13271,#13272,#13273,#13274,#13275,#13276,#13277,#13278,#13279,
#13280,#13281,#13282,#13283,#13284,#13285,#13286,#13287,#13288,#13289,#13290,
#13291,#13292,#13293,#13294,#13295,#13296,#13297,#13298,#13299,#13300,#13301,
#13302,#13303,#13304,#13305,#13306,#13307,#13308,#13309,#13310,#13311,#13312,
#13313,#13314,#13315,#13316,#13317,#13318),(#13319,#13320,#13321,#13322,
#13323,#13324,#13325,#13326,#13327,#13328,#13329,#13330,#13331,#13332,#13333,
#13334,#13335,#13336,#13337,#13338,#13339,#13340,#13341,#13342,#13343,#13344,
#13345,#13346,#13347,#13348,#13349,#13350,#13351,#13352,#13353,#13354,#13355,
#13356,#13357,#13358,#13359,#13360,#13361,#13362,#13363,#13364,#13365,#13366,
#13367,#13368,#13369,#13370,#13371,#13372,#13373,#13374,#13375,#13376,#13377,
#13378,#13379,#13380,#13381,#13382,#13383,#13384,#13385,#13386,#13387,#13388,
#13389,#13390,#13391,#13392,#13393,#13394,#13395,#13396,#13397,#13398,#13399,
#13400,#13401,#13402,#13403,#13404,#13405,#13406,#13407,#13408,#13409,#13410,
#13411,#13412,#13413,#13414,#13415,#13416,#13417,#13418,#13419,#13420,#13421,
#13422),(#13423,#13424,#13425,#13426,#13427,#13428,#13429,#13430,#13431,
#13432,#13433,#13434,#13435,#13436,#13437,#13438,#13439,#13440,#13441,#13442,
#13443,#13444,#13445,#13446,#13447,#13448,#13449,#13450,#13451,#13452,#13453,
#13454,#13455,#13456,#13457,#13458,#13459,#13460,#13461,#13462,#13463,#13464,
#13465,#13466,#13467,#13468,#13469,#13470,#13471,#13472,#13473,#13474,#13475,
#13476,#13477,#13478,#13479,#13480,#13481,#13482,#13483,#13484,#13485,#13486,
#13487,#13488,#13489,#13490,#13491,#13492,#13493,#13494,#13495,#13496,#13497,
#13498,#13499,#13500,#13501,#13502,#13503,#13504,#13505,#13506,#13507,#13508,
#13509,#13510,#13511,#13512,#13513,#13514,#13515,#13516,#13517,#13518,#13519,
#13520,#13521,#13522,#13523,#13524,#13525,#13526)),.UNSPECIFIED.,.F.,.F.,
 .F.,(4,4),(4,1,1,1,1,1,1,1,1,1,1,1,1,1,1,1,1,1,1,1,1,1,1,1,1,1,1,1,1,1,
1,1,1,1,1,1,1,1,1,1,1,1,1,1,1,1,1,1,1,1,1,1,1,1,1,1,1,1,1,1,1,1,1,1,1,1,
1,1,1,1,1,1,1,1,1,1,1,1,1,1,1,1,1,1,1,1,1,1,1,1,1,1,1,1,1,1,1,1,1,1,1,4),
(0.,0.0448889834294942),(14.3981410127769,15.3956695472135,16.3931980816501,
17.3907266160867,18.3882551505233,19.3857836849599,20.3833122193965,21.3808407538331,
22.3783692882697,23.3758978227063,24.3734263571429,25.3709548915795,26.3684834260161,
27.3660119604527,28.3635404948893,29.3610690293259,30.3585975637625,31.3561260981991,
32.3536546326357,33.3511831670723,34.3487117015089,35.3462402359455,36.3437687703821,
37.3412973048187,38.3388258392553,39.3363543736919,40.3338829081285,41.3314114425651,
42.3289399770017,43.3264685114383,44.3239970458749,45.3215255803115,46.3190541147481,
47.3165826491847,48.3141111836213,49.3116397180579,50.3091682524945,51.3066967869311,
52.3042253213677,53.3017538558043,54.2992823902409,55.2968109246775,56.294339459114,
57.2918679935507,58.2893965279873,59.2869250624238,60.2844535968605,61.281982131297,
62.2795106657336,63.2770392001703,64.2745677346068,65.2720962690434,66.26962480348,
67.2671533379167,68.2646818723532,69.2622104067898,70.2597389412264,71.257267475663,
72.2547960100996,73.2523245445362,74.2498530789728,75.2473816134094,76.244910147846,
77.2424386822826,78.2399672167192,79.2374957511558,80.2350242855924,81.232552820029,
82.2300813544656,83.2276098889022,84.2251384233388,85.2226669577754,86.220195492212,
87.2177240266486,88.2152525610852,89.2127810955218,90.2103096299584,91.207838164395,
92.2053666988316,93.2028952332682,94.2004237677048,95.1979523021414,96.195480836578,
97.1930093710146,98.1905379054512,99.1880664398878,100.185594974324,101.183123508761,
102.180652043198,103.178180577634,104.175709112071,105.173237646507,106.170766180944,
107.168294715381,108.165823249817,109.163351784254,110.16088031869,111.158408853127,
112.155937387564,113.153465922,114.150994456437,115.148522990873),
 .UNSPECIFIED.);
#121=B_SPLINE_SURFACE_WITH_KNOTS('',3,3,((#14592,#14593,#14594,#14595,#14596,
#14597,#14598,#14599,#14600,#14601,#14602,#14603,#14604,#14605,#14606,#14607,
#14608,#14609,#14610,#14611,#14612,#14613,#14614,#14615,#14616,#14617,#14618,
#14619,#14620,#14621,#14622,#14623,#14624,#14625,#14626,#14627,#14628,#14629,
#14630,#14631,#14632,#14633,#14634,#14635,#14636,#14637,#14638,#14639,#14640,
#14641,#14642,#14643,#14644,#14645,#14646,#14647,#14648,#14649,#14650,#14651,
#14652,#14653,#14654,#14655,#14656,#14657,#14658,#14659),(#14660,#14661,
#14662,#14663,#14664,#14665,#14666,#14667,#14668,#14669,#14670,#14671,#14672,
#14673,#14674,#14675,#14676,#14677,#14678,#14679,#14680,#14681,#14682,#14683,
#14684,#14685,#14686,#14687,#14688,#14689,#14690,#14691,#14692,#14693,#14694,
#14695,#14696,#14697,#14698,#14699,#14700,#14701,#14702,#14703,#14704,#14705,
#14706,#14707,#14708,#14709,#14710,#14711,#14712,#14713,#14714,#14715,#14716,
#14717,#14718,#14719,#14720,#14721,#14722,#14723,#14724,#14725,#14726,#14727),
(#14728,#14729,#14730,#14731,#14732,#14733,#14734,#14735,#14736,#14737,
#14738,#14739,#14740,#14741,#14742,#14743,#14744,#14745,#14746,#14747,#14748,
#14749,#14750,#14751,#14752,#14753,#14754,#14755,#14756,#14757,#14758,#14759,
#14760,#14761,#14762,#14763,#14764,#14765,#14766,#14767,#14768,#14769,#14770,
#14771,#14772,#14773,#14774,#14775,#14776,#14777,#14778,#14779,#14780,#14781,
#14782,#14783,#14784,#14785,#14786,#14787,#14788,#14789,#14790,#14791,#14792,
#14793,#14794,#14795),(#14796,#14797,#14798,#14799,#14800,#14801,#14802,
#14803,#14804,#14805,#14806,#14807,#14808,#14809,#14810,#14811,#14812,#14813,
#14814,#14815,#14816,#14817,#14818,#14819,#14820,#14821,#14822,#14823,#14824,
#14825,#14826,#14827,#14828,#14829,#14830,#14831,#14832,#14833,#14834,#14835,
#14836,#14837,#14838,#14839,#14840,#14841,#14842,#14843,#14844,#14845,#14846,
#14847,#14848,#14849,#14850,#14851,#14852,#14853,#14854,#14855,#14856,#14857,
#14858,#14859,#14860,#14861,#14862,#14863)),.UNSPECIFIED.,.F.,.F.,.F.,(4,
4),(4,1,1,1,1,1,1,1,1,1,1,1,1,1,1,1,1,1,1,1,1,1,1,1,1,1,1,1,1,1,1,1,1,1,
1,1,1,1,1,1,1,1,1,1,1,1,1,1,1,1,1,1,1,1,1,1,1,1,1,1,1,1,1,1,1,4),(0.,0.0642013499338864),
(11.8589888623078,12.8566626771512,13.8543364919947,14.8520103068381,15.8496841216816,
16.8473579365251,17.8450317513685,18.842705566212,19.8403793810554,20.8380531958989,
21.8357270107423,22.8334008255858,23.8310746404292,24.8287484552727,25.8264222701161,
26.8240960849596,27.821769899803,28.8194437146465,29.8171175294899,30.8147913443334,
31.8124651591768,32.8101389740203,33.8078127888637,34.8054866037072,35.8031604185506,
36.8008342333941,37.7985080482375,38.796181863081,39.7938556779244,40.7915294927679,
41.7892033076113,42.7868771224548,43.7845509372982,44.7822247521417,45.7798985669851,
46.7775723818286,47.775246196672,48.7729200115155,49.7705938263589,50.7682676412024,
51.7659414560458,52.7636152708893,53.7612890857327,54.7589629005762,55.7566367154196,
56.7543105302631,57.7519843451065,58.74965815995,59.7473319747934,60.7450057896369,
61.7426796044803,62.7403534193238,63.7380272341672,64.7357010490107,65.7333748638542,
66.7310486786976,67.728722493541,68.7263963083845,69.7240701232279,70.7217439380714,
71.7194177529149,72.7170915677583,73.7147653826018,74.7124391974452,75.7101130122887,
76.7077868271321),.UNSPECIFIED.);
#122=B_SPLINE_SURFACE_WITH_KNOTS('',3,3,((#15080,#15081,#15082,#15083,#15084,
#15085,#15086,#15087,#15088,#15089,#15090,#15091,#15092,#15093,#15094,#15095,
#15096,#15097,#15098,#15099,#15100,#15101,#15102,#15103,#15104,#15105,#15106,
#15107,#15108,#15109,#15110,#15111,#15112,#15113,#15114,#15115,#15116,#15117,
#15118,#15119,#15120,#15121,#15122,#15123,#15124,#15125,#15126,#15127,#15128,
#15129,#15130,#15131,#15132,#15133,#15134,#15135,#15136,#15137,#15138,#15139,
#15140,#15141,#15142,#15143,#15144,#15145,#15146,#15147),(#15148,#15149,
#15150,#15151,#15152,#15153,#15154,#15155,#15156,#15157,#15158,#15159,#15160,
#15161,#15162,#15163,#15164,#15165,#15166,#15167,#15168,#15169,#15170,#15171,
#15172,#15173,#15174,#15175,#15176,#15177,#15178,#15179,#15180,#15181,#15182,
#15183,#15184,#15185,#15186,#15187,#15188,#15189,#15190,#15191,#15192,#15193,
#15194,#15195,#15196,#15197,#15198,#15199,#15200,#15201,#15202,#15203,#15204,
#15205,#15206,#15207,#15208,#15209,#15210,#15211,#15212,#15213,#15214,#15215),
(#15216,#15217,#15218,#15219,#15220,#15221,#15222,#15223,#15224,#15225,
#15226,#15227,#15228,#15229,#15230,#15231,#15232,#15233,#15234,#15235,#15236,
#15237,#15238,#15239,#15240,#15241,#15242,#15243,#15244,#15245,#15246,#15247,
#15248,#15249,#15250,#15251,#15252,#15253,#15254,#15255,#15256,#15257,#15258,
#15259,#15260,#15261,#15262,#15263,#15264,#15265,#15266,#15267,#15268,#15269,
#15270,#15271,#15272,#15273,#15274,#15275,#15276,#15277,#15278,#15279,#15280,
#15281,#15282,#15283),(#15284,#15285,#15286,#15287,#15288,#15289,#15290,
#15291,#15292,#15293,#15294,#15295,#15296,#15297,#15298,#15299,#15300,#15301,
#15302,#15303,#15304,#15305,#15306,#15307,#15308,#15309,#15310,#15311,#15312,
#15313,#15314,#15315,#15316,#15317,#15318,#15319,#15320,#15321,#15322,#15323,
#15324,#15325,#15326,#15327,#15328,#15329,#15330,#15331,#15332,#15333,#15334,
#15335,#15336,#15337,#15338,#15339,#15340,#15341,#15342,#15343,#15344,#15345,
#15346,#15347,#15348,#15349,#15350,#15351)),.UNSPECIFIED.,.F.,.F.,.F.,(4,
4),(4,1,1,1,1,1,1,1,1,1,1,1,1,1,1,1,1,1,1,1,1,1,1,1,1,1,1,1,1,1,1,1,1,1,
1,1,1,1,1,1,1,1,1,1,1,1,1,1,1,1,1,1,1,1,1,1,1,1,1,1,1,1,1,1,1,4),(0.,0.0642013499338864),
(14.3984001269718,15.3960739418153,16.3937477566587,17.3914215715022,18.3890953863456,
19.3867692011891,20.3844430160325,21.382116830876,22.3797906457194,23.3774644605629,
24.3751382754063,25.3728120902498,26.3704859050932,27.3681597199367,28.3658335347801,
29.3635073496236,30.361181164467,31.3588549793105,32.3565287941539,33.3542026089974,
34.3518764238408,35.3495502386843,36.3472240535278,37.3448978683712,38.3425716832147,
39.3402454980581,40.3379193129016,41.335593127745,42.3332669425885,43.3309407574319,
44.3286145722754,45.3262883871188,46.3239622019623,47.3216360168057,48.3193098316492,
49.3169836464926,50.3146574613361,51.3123312761795,52.310005091023,53.3076789058664,
54.3053527207099,55.3030265355533,56.3007003503968,57.2983741652402,58.2960479800837,
59.2937217949271,60.2913956097706,61.289069424614,62.2867432394575,63.2844170543009,
64.2820908691444,65.2797646839878,66.2774384988313,67.2751123136747,68.2727861285182,
69.2704599433616,70.2681337582051,71.2658075730485,72.263481387892,73.2611552027354,
74.2588290175789,75.2565028324223,76.2541766472658,77.2518504621092,78.2495242769527,
79.2471980917962),.UNSPECIFIED.);
#123=B_SPLINE_SURFACE_WITH_KNOTS('',3,3,((#16881,#16882,#16883,#16884,#16885,
#16886,#16887,#16888,#16889,#16890,#16891,#16892,#16893,#16894,#16895,#16896,
#16897,#16898,#16899,#16900,#16901,#16902,#16903,#16904,#16905,#16906,#16907,
#16908,#16909,#16910,#16911,#16912,#16913,#16914,#16915,#16916,#16917,#16918,
#16919,#16920,#16921,#16922,#16923,#16924,#16925,#16926,#16927,#16928,#16929,
#16930,#16931,#16932,#16933),(#16934,#16935,#16936,#16937,#16938,#16939,
#16940,#16941,#16942,#16943,#16944,#16945,#16946,#16947,#16948,#16949,#16950,
#16951,#16952,#16953,#16954,#16955,#16956,#16957,#16958,#16959,#16960,#16961,
#16962,#16963,#16964,#16965,#16966,#16967,#16968,#16969,#16970,#16971,#16972,
#16973,#16974,#16975,#16976,#16977,#16978,#16979,#16980,#16981,#16982,#16983,
#16984,#16985,#16986),(#16987,#16988,#16989,#16990,#16991,#16992,#16993,
#16994,#16995,#16996,#16997,#16998,#16999,#17000,#17001,#17002,#17003,#17004,
#17005,#17006,#17007,#17008,#17009,#17010,#17011,#17012,#17013,#17014,#17015,
#17016,#17017,#17018,#17019,#17020,#17021,#17022,#17023,#17024,#17025,#17026,
#17027,#17028,#17029,#17030,#17031,#17032,#17033,#17034,#17035,#17036,#17037,
#17038,#17039),(#17040,#17041,#17042,#17043,#17044,#17045,#17046,#17047,
#17048,#17049,#17050,#17051,#17052,#17053,#17054,#17055,#17056,#17057,#17058,
#17059,#17060,#17061,#17062,#17063,#17064,#17065,#17066,#17067,#17068,#17069,
#17070,#17071,#17072,#17073,#17074,#17075,#17076,#17077,#17078,#17079,#17080,
#17081,#17082,#17083,#17084,#17085,#17086,#17087,#17088,#17089,#17090,#17091,
#17092)),.UNSPECIFIED.,.F.,.F.,.F.,(4,4),(4,1,1,1,1,1,1,1,1,1,1,1,1,1,1,
1,1,1,1,1,1,1,1,1,1,1,1,1,1,1,1,1,1,1,1,1,1,1,1,1,1,1,1,1,1,1,1,1,1,1,4),
(0.,0.0658467982010768),(13.9508069857623,14.9507739156503,15.9507408455384,
16.9507077754264,17.9506747053144,18.9506416352025,19.9506085650905,20.9505754949786,
21.9505424248666,22.9505093547546,23.9504762846427,24.9504432145307,25.9504101444187,
26.9503770743068,27.9503440041948,28.9503109340829,29.9502778639709,30.9502447938589,
31.950211723747,32.950178653635,33.950145583523,34.9501125134111,35.9500794432991,
36.9500463731871,37.9500133030752,38.9499802329632,39.9499471628512,40.9499140927393,
41.9498810226273,42.9498479525154,43.9498148824034,44.9497818122914,45.9497487421795,
46.9497156720675,47.9496826019555,48.9496495318436,49.9496164617316,50.9495833916196,
51.9495503215077,52.9495172513957,53.9494841812838,54.9494511111718,55.9494180410598,
56.9493849709479,57.9493519008359,58.9493188307239,59.949285760612,60.9492526905,
61.949219620388,62.9491865502761,63.9491534801641),.UNSPECIFIED.);
#124=B_SPLINE_SURFACE_WITH_KNOTS('',3,3,((#17265,#17266,#17267,#17268,#17269,
#17270,#17271,#17272,#17273,#17274,#17275,#17276,#17277,#17278,#17279,#17280,
#17281,#17282,#17283,#17284,#17285,#17286,#17287,#17288,#17289,#17290,#17291,
#17292,#17293,#17294,#17295,#17296,#17297,#17298,#17299,#17300,#17301,#17302,
#17303,#17304,#17305,#17306,#17307,#17308,#17309,#17310,#17311,#17312,#17313,
#17314,#17315),(#17316,#17317,#17318,#17319,#17320,#17321,#17322,#17323,
#17324,#17325,#17326,#17327,#17328,#17329,#17330,#17331,#17332,#17333,#17334,
#17335,#17336,#17337,#17338,#17339,#17340,#17341,#17342,#17343,#17344,#17345,
#17346,#17347,#17348,#17349,#17350,#17351,#17352,#17353,#17354,#17355,#17356,
#17357,#17358,#17359,#17360,#17361,#17362,#17363,#17364,#17365,#17366),
(#17367,#17368,#17369,#17370,#17371,#17372,#17373,#17374,#17375,#17376,
#17377,#17378,#17379,#17380,#17381,#17382,#17383,#17384,#17385,#17386,#17387,
#17388,#17389,#17390,#17391,#17392,#17393,#17394,#17395,#17396,#17397,#17398,
#17399,#17400,#17401,#17402,#17403,#17404,#17405,#17406,#17407,#17408,#17409,
#17410,#17411,#17412,#17413,#17414,#17415,#17416,#17417),(#17418,#17419,
#17420,#17421,#17422,#17423,#17424,#17425,#17426,#17427,#17428,#17429,#17430,
#17431,#17432,#17433,#17434,#17435,#17436,#17437,#17438,#17439,#17440,#17441,
#17442,#17443,#17444,#17445,#17446,#17447,#17448,#17449,#17450,#17451,#17452,
#17453,#17454,#17455,#17456,#17457,#17458,#17459,#17460,#17461,#17462,#17463,
#17464,#17465,#17466,#17467,#17468)),.UNSPECIFIED.,.F.,.F.,.F.,(4,4),(4,
1,1,1,1,1,1,1,1,1,1,1,1,1,1,1,1,1,1,1,1,1,1,1,1,1,1,1,1,1,1,1,1,1,1,1,1,
1,1,1,1,1,1,1,1,1,1,1,4),(0.,0.0658467982010768),(12.7118898652542,13.7104254552436,
14.7089610452331,15.7074966352225,16.7060322252119,17.7045678152014,18.7031034051908,
19.7016389951802,20.7001745851697,21.6987101751591,22.6972457651485,23.695781355138,
24.6943169451274,25.6928525351168,26.6913881251062,27.6899237150957,28.6884593050851,
29.6869948950745,30.685530485064,31.6840660750534,32.6826016650428,33.6811372550323,
34.6796728450217,35.6782084350111,36.6767440250006,37.67527961499,38.6738152049794,
39.6723507949688,40.6708863849583,41.6694219749477,42.6679575649371,43.6664931549266,
44.665028744916,45.6635643349054,46.6620999248949,47.6606355148843,48.6591711048737,
49.6577066948632,50.6562422848526,51.654777874842,52.6533134648314,53.6518490548209,
54.6503846448103,55.6489202347997,56.6474558247892,57.6459914147786,58.644527004768,
59.6430625947575,60.6415981847469),.UNSPECIFIED.);
#125=B_SPLINE_SURFACE_WITH_KNOTS('',3,3,((#18814,#18815,#18816,#18817,#18818,
#18819,#18820,#18821,#18822,#18823,#18824,#18825,#18826,#18827,#18828,#18829,
#18830,#18831,#18832,#18833,#18834,#18835,#18836,#18837,#18838,#18839,#18840,
#18841,#18842,#18843,#18844,#18845,#18846,#18847,#18848,#18849,#18850,#18851,
#18852,#18853,#18854,#18855,#18856,#18857,#18858,#18859,#18860,#18861,#18862,
#18863,#18864,#18865,#18866,#18867,#18868,#18869,#18870,#18871,#18872,#18873,
#18874,#18875,#18876,#18877,#18878,#18879,#18880,#18881,#18882,#18883,#18884,
#18885,#18886,#18887,#18888,#18889,#18890,#18891,#18892,#18893,#18894,#18895,
#18896,#18897,#18898,#18899,#18900,#18901),(#18902,#18903,#18904,#18905,
#18906,#18907,#18908,#18909,#18910,#18911,#18912,#18913,#18914,#18915,#18916,
#18917,#18918,#18919,#18920,#18921,#18922,#18923,#18924,#18925,#18926,#18927,
#18928,#18929,#18930,#18931,#18932,#18933,#18934,#18935,#18936,#18937,#18938,
#18939,#18940,#18941,#18942,#18943,#18944,#18945,#18946,#18947,#18948,#18949,
#18950,#18951,#18952,#18953,#18954,#18955,#18956,#18957,#18958,#18959,#18960,
#18961,#18962,#18963,#18964,#18965,#18966,#18967,#18968,#18969,#18970,#18971,
#18972,#18973,#18974,#18975,#18976,#18977,#18978,#18979,#18980,#18981,#18982,
#18983,#18984,#18985,#18986,#18987,#18988,#18989),(#18990,#18991,#18992,
#18993,#18994,#18995,#18996,#18997,#18998,#18999,#19000,#19001,#19002,#19003,
#19004,#19005,#19006,#19007,#19008,#19009,#19010,#19011,#19012,#19013,#19014,
#19015,#19016,#19017,#19018,#19019,#19020,#19021,#19022,#19023,#19024,#19025,
#19026,#19027,#19028,#19029,#19030,#19031,#19032,#19033,#19034,#19035,#19036,
#19037,#19038,#19039,#19040,#19041,#19042,#19043,#19044,#19045,#19046,#19047,
#19048,#19049,#19050,#19051,#19052,#19053,#19054,#19055,#19056,#19057,#19058,
#19059,#19060,#19061,#19062,#19063,#19064,#19065,#19066,#19067,#19068,#19069,
#19070,#19071,#19072,#19073,#19074,#19075,#19076,#19077),(#19078,#19079,
#19080,#19081,#19082,#19083,#19084,#19085,#19086,#19087,#19088,#19089,#19090,
#19091,#19092,#19093,#19094,#19095,#19096,#19097,#19098,#19099,#19100,#19101,
#19102,#19103,#19104,#19105,#19106,#19107,#19108,#19109,#19110,#19111,#19112,
#19113,#19114,#19115,#19116,#19117,#19118,#19119,#19120,#19121,#19122,#19123,
#19124,#19125,#19126,#19127,#19128,#19129,#19130,#19131,#19132,#19133,#19134,
#19135,#19136,#19137,#19138,#19139,#19140,#19141,#19142,#19143,#19144,#19145,
#19146,#19147,#19148,#19149,#19150,#19151,#19152,#19153,#19154,#19155,#19156,
#19157,#19158,#19159,#19160,#19161,#19162,#19163,#19164,#19165)),
 .UNSPECIFIED.,.F.,.F.,.F.,(4,4),(4,1,1,1,1,1,1,1,1,1,1,1,1,1,1,1,1,1,1,
1,1,1,1,1,1,1,1,1,1,1,1,1,1,1,1,1,1,1,1,1,1,1,1,1,1,1,1,1,1,1,1,1,1,1,1,
1,1,1,1,1,1,1,1,1,1,1,1,1,1,1,1,1,1,1,1,1,1,1,1,1,1,1,1,1,1,4),(0.,0.0460148164544132),
(11.6154215191106,12.6127583869031,13.6100952546957,14.6074321224883,15.6047689902808,
16.6021058580734,17.599442725866,18.5967795936585,19.5941164614511,20.5914533292437,
21.5887901970362,22.5861270648288,23.5834639326213,24.5808008004139,25.5781376682065,
26.575474535999,27.5728114037916,28.5701482715842,29.5674851393767,30.5648220071693,
31.5621588749619,32.5594957427544,33.556832610547,34.5541694783396,35.5515063461321,
36.5488432139247,37.5461800817173,38.5435169495098,39.5408538173024,40.538190685095,
41.5355275528875,42.5328644206801,43.5302012884726,44.5275381562652,45.5248750240578,
46.5222118918503,47.5195487596429,48.5168856274355,49.514222495228,50.5115593630206,
51.5088962308132,52.5062330986057,53.5035699663983,54.5009068341909,55.4982437019834,
56.495580569776,57.4929174375686,58.4902543053611,59.4875911731537,60.4849280409463,
61.4822649087388,62.4796017765314,63.4769386443239,64.4742755121165,65.4716123799091,
66.4689492477016,67.4662861154942,68.4636229832868,69.4609598510793,70.4582967188719,
71.4556335866645,72.452970454457,73.4503073222496,74.4476441900422,75.4449810578347,
76.4423179256273,77.4396547934198,78.4369916612124,79.434328529005,80.4316653967976,
81.4290022645901,82.4263391323827,83.4236760001752,84.4210128679678,85.4183497357604,
86.4156866035529,87.4130234713455,88.4103603391381,89.4076972069306,90.4050340747232,
91.4023709425158,92.3997078103083,93.3970446781009,94.3943815458935,95.391718413686,
96.3890552814786),.UNSPECIFIED.);
#126=B_SPLINE_SURFACE_WITH_KNOTS('',3,3,((#19288,#19289,#19290,#19291,#19292,
#19293,#19294,#19295,#19296,#19297,#19298,#19299,#19300,#19301,#19302,#19303,
#19304,#19305,#19306,#19307,#19308,#19309,#19310,#19311,#19312,#19313,#19314,
#19315,#19316,#19317,#19318,#19319,#19320,#19321,#19322,#19323,#19324,#19325,
#19326,#19327,#19328,#19329,#19330,#19331,#19332,#19333,#19334,#19335,#19336,
#19337,#19338,#19339,#19340,#19341,#19342,#19343,#19344,#19345,#19346,#19347,
#19348,#19349,#19350,#19351,#19352,#19353,#19354,#19355,#19356,#19357,#19358,
#19359,#19360,#19361,#19362,#19363,#19364,#19365,#19366,#19367,#19368,#19369,
#19370,#19371,#19372,#19373,#19374,#19375,#19376,#19377),(#19378,#19379,
#19380,#19381,#19382,#19383,#19384,#19385,#19386,#19387,#19388,#19389,#19390,
#19391,#19392,#19393,#19394,#19395,#19396,#19397,#19398,#19399,#19400,#19401,
#19402,#19403,#19404,#19405,#19406,#19407,#19408,#19409,#19410,#19411,#19412,
#19413,#19414,#19415,#19416,#19417,#19418,#19419,#19420,#19421,#19422,#19423,
#19424,#19425,#19426,#19427,#19428,#19429,#19430,#19431,#19432,#19433,#19434,
#19435,#19436,#19437,#19438,#19439,#19440,#19441,#19442,#19443,#19444,#19445,
#19446,#19447,#19448,#19449,#19450,#19451,#19452,#19453,#19454,#19455,#19456,
#19457,#19458,#19459,#19460,#19461,#19462,#19463,#19464,#19465,#19466,#19467),
(#19468,#19469,#19470,#19471,#19472,#19473,#19474,#19475,#19476,#19477,
#19478,#19479,#19480,#19481,#19482,#19483,#19484,#19485,#19486,#19487,#19488,
#19489,#19490,#19491,#19492,#19493,#19494,#19495,#19496,#19497,#19498,#19499,
#19500,#19501,#19502,#19503,#19504,#19505,#19506,#19507,#19508,#19509,#19510,
#19511,#19512,#19513,#19514,#19515,#19516,#19517,#19518,#19519,#19520,#19521,
#19522,#19523,#19524,#19525,#19526,#19527,#19528,#19529,#19530,#19531,#19532,
#19533,#19534,#19535,#19536,#19537,#19538,#19539,#19540,#19541,#19542,#19543,
#19544,#19545,#19546,#19547,#19548,#19549,#19550,#19551,#19552,#19553,#19554,
#19555,#19556,#19557),(#19558,#19559,#19560,#19561,#19562,#19563,#19564,
#19565,#19566,#19567,#19568,#19569,#19570,#19571,#19572,#19573,#19574,#19575,
#19576,#19577,#19578,#19579,#19580,#19581,#19582,#19583,#19584,#19585,#19586,
#19587,#19588,#19589,#19590,#19591,#19592,#19593,#19594,#19595,#19596,#19597,
#19598,#19599,#19600,#19601,#19602,#19603,#19604,#19605,#19606,#19607,#19608,
#19609,#19610,#19611,#19612,#19613,#19614,#19615,#19616,#19617,#19618,#19619,
#19620,#19621,#19622,#19623,#19624,#19625,#19626,#19627,#19628,#19629,#19630,
#19631,#19632,#19633,#19634,#19635,#19636,#19637,#19638,#19639,#19640,#19641,
#19642,#19643,#19644,#19645,#19646,#19647)),.UNSPECIFIED.,.F.,.F.,.F.,(4,
4),(4,1,1,1,1,1,1,1,1,1,1,1,1,1,1,1,1,1,1,1,1,1,1,1,1,1,1,1,1,1,1,1,1,1,
1,1,1,1,1,1,1,1,1,1,1,1,1,1,1,1,1,1,1,1,1,1,1,1,1,1,1,1,1,1,1,1,1,1,1,1,
1,1,1,1,1,1,1,1,1,1,1,1,1,1,1,1,1,4),(0.,0.0460148164544132),(8.31058692273971,
9.30873374912645,10.3068805755132,11.3050274018999,12.3031742282867,13.3013210546734,
14.2994678810601,15.2976147074469,16.2957615338336,17.2939083602203,18.2920551866071,
19.2902020129938,20.2883488393806,21.2864956657673,22.284642492154,23.2827893185408,
24.2809361449275,25.2790829713142,26.277229797701,27.2753766240877,28.2735234504744,
29.2716702768612,30.2698171032479,31.2679639296347,32.2661107560214,33.2642575824081,
34.2624044087949,35.2605512351816,36.2586980615683,37.2568448879551,38.2549917143418,
39.2531385407286,40.2512853671153,41.249432193502,42.2475790198888,43.2457258462755,
44.2438726726622,45.242019499049,46.2401663254357,47.2383131518225,48.2364599782092,
49.2346068045959,50.2327536309827,51.2309004573694,52.2290472837561,53.2271941101429,
54.2253409365296,55.2234877629163,56.2216345893031,57.2197814156898,58.2179282420766,
59.2160750684633,60.21422189485,61.2123687212368,62.2105155476235,63.2086623740102,
64.206809200397,65.2049560267837,66.2031028531704,67.2012496795572,68.1993965059439,
69.1975433323307,70.1956901587174,71.1938369851041,72.1919838114909,73.1901306378776,
74.1882774642643,75.1864242906511,76.1845711170378,77.1827179434245,78.1808647698113,
79.179011596198,80.1771584225848,81.1753052489715,82.1734520753582,83.171598901745,
84.1697457281317,85.1678925545184,86.1660393809052,87.1641862072919,88.1623330336787,
89.1604798600654,90.1586266864521,91.1567735128389,92.1549203392256,93.1530671656123,
94.1512139919991,95.1493608183858),.UNSPECIFIED.);
#127=B_SPLINE_CURVE_WITH_KNOTS('',3,(#8912,#8913,#8914,#8915,#8916,#8917,
#8918,#8919,#8920,#8921,#8922,#8923,#8924,#8925,#8926,#8927,#8928,#8929,
#8930),.UNSPECIFIED.,.F.,.F.,(4,3,3,3,3,3,4),(95.5576018628658,95.7627393059135,
96.7602678403501,97.7577963747867,98.7553249092233,99.7528534436599,100.750381978097),
 .UNSPECIFIED.);
#128=B_SPLINE_CURVE_WITH_KNOTS('',3,(#8934,#8935,#8936,#8937),
 .UNSPECIFIED.,.F.,.F.,(4,4),(-98.7357691128221,-98.0941628713861),
 .UNSPECIFIED.);
#129=B_SPLINE_CURVE_WITH_KNOTS('',3,(#8941,#8942,#8943,#8944,#8945,#8946,
#8947,#8948,#8949,#8950,#8951,#8952,#8953,#8954,#8955,#8956,#8957,#8958,
#8959,#8960,#8961,#8962),.UNSPECIFIED.,.F.,.F.,(4,3,3,3,3,3,3,4),(-98.0941628713861,
-97.7577963747867,-96.7602678403501,-95.7627393059135,-94.7652107714769,
-93.7676822370403,-92.7701537026037,-91.8109775642065),.UNSPECIFIED.);
#130=B_SPLINE_CURVE_WITH_KNOTS('',3,(#8967,#8968,#8969,#8970,#8971,#8972,
#8973,#8974,#8975,#8976,#8977,#8978,#8979,#8980,#8981,#8982,#8983,#8984,
#8985,#8986,#8987,#8988),.UNSPECIFIED.,.F.,.F.,(4,3,3,3,3,3,3,4),(89.2744165556862,
89.7775680992939,90.7750966337306,91.7726251681671,92.7701537026037,93.7676822370403,
94.7652107714769,95.5576018628658),.UNSPECIFIED.);
#131=B_SPLINE_CURVE_WITH_KNOTS('',3,(#8989,#8990,#8991,#8992,#8993,#8994,
#8995,#8996,#8997,#8998,#8999,#9000,#9001,#9002,#9003,#9004,#9005,#9006,
#9007,#9008,#9009,#9010,#9011,#9012,#9013),.UNSPECIFIED.,.F.,.F.,(4,3,3,
3,3,3,3,3,4),(-91.8109775642065,-91.7726251681671,-90.7750966337305,-89.7775680992939,
-88.7800395648573,-87.7825110304207,-86.7849824959842,-85.7874539615476,
-85.5277922570269),.UNSPECIFIED.);
#132=B_SPLINE_CURVE_WITH_KNOTS('',3,(#9018,#9019,#9020,#9021,#9022,#9023,
#9024,#9025,#9026,#9027,#9028,#9029,#9030,#9031,#9032,#9033,#9034,#9035,
#9036,#9037,#9038,#9039),.UNSPECIFIED.,.F.,.F.,(4,3,3,3,3,3,3,4),(82.9912312485066,
83.7923968926743,84.7899254271109,85.7874539615476,86.7849824959841,87.7825110304207,
88.7800395648573,89.2744165556862),.UNSPECIFIED.);
#133=B_SPLINE_CURVE_WITH_KNOTS('',3,(#9040,#9041,#9042,#9043,#9044,#9045,
#9046,#9047,#9048,#9049,#9050,#9051,#9052,#9053,#9054,#9055,#9056,#9057,
#9058,#9059,#9060,#9061),.UNSPECIFIED.,.F.,.F.,(4,3,3,3,3,3,3,4),(-85.5277922570269,
-84.789925427111,-83.7923968926743,-82.7948683582377,-81.7973398238011,
-80.7998112893646,-79.8022827549279,-79.2446069498473),.UNSPECIFIED.);
#134=B_SPLINE_CURVE_WITH_KNOTS('',3,(#9066,#9067,#9068,#9069,#9070,#9071,
#9072,#9073,#9074,#9075,#9076,#9077,#9078,#9079,#9080,#9081,#9082,#9083,
#9084,#9085,#9086,#9087,#9088,#9089,#9090),.UNSPECIFIED.,.F.,.F.,(4,3,3,
3,3,3,3,3,4),(76.708045941327,76.8096971516181,77.8072256860547,78.8047542204914,
79.8022827549279,80.7998112893646,81.7973398238011,82.7948683582377,82.9912312485066),
 .UNSPECIFIED.);
#135=B_SPLINE_CURVE_WITH_KNOTS('',3,(#9091,#9092,#9093,#9094,#9095,#9096,
#9097,#9098,#9099,#9100,#9101,#9102,#9103,#9104,#9105,#9106,#9107,#9108,
#9109,#9110,#9111,#9112),.UNSPECIFIED.,.F.,.F.,(4,3,3,3,3,3,3,4),(-79.2446069498473,
-78.8047542204913,-77.8072256860547,-76.8096971516181,-75.8121686171815,
-74.8146400827449,-73.8171115483083,-72.9614216426677),.UNSPECIFIED.);
#136=B_SPLINE_CURVE_WITH_KNOTS('',3,(#9117,#9118,#9119,#9120,#9121,#9122,
#9123,#9124,#9125,#9126,#9127,#9128,#9129,#9130,#9131,#9132,#9133,#9134,
#9135,#9136,#9137,#9138),.UNSPECIFIED.,.F.,.F.,(4,3,3,3,3,3,3,4),(70.4248606341474,
70.8245259449985,71.8220544794352,72.8195830138717,73.8171115483084,74.8146400827449,
75.8121686171816,76.708045941327),.UNSPECIFIED.);
#137=B_SPLINE_CURVE_WITH_KNOTS('',3,(#9139,#9140,#9141,#9142,#9143,#9144,
#9145,#9146,#9147,#9148,#9149,#9150,#9151,#9152,#9153,#9154,#9155,#9156,
#9157,#9158,#9159,#9160,#9161,#9162,#9163),.UNSPECIFIED.,.F.,.F.,(4,3,3,
3,3,3,3,3,4),(-72.9614216426677,-72.8195830138717,-71.8220544794352,-70.8245259449986,
-69.8269974105619,-68.8294688761253,-67.8319403416887,-66.8344118072522,
-66.6782363354881),.UNSPECIFIED.);
#138=B_SPLINE_CURVE_WITH_KNOTS('',3,(#9168,#9169,#9170,#9171,#9172,#9173,
#9174,#9175,#9176,#9177,#9178,#9179,#9180,#9181,#9182,#9183,#9184,#9185,
#9186,#9187,#9188,#9189),.UNSPECIFIED.,.F.,.F.,(4,3,3,3,3,3,3,4),(64.1416753269678,
64.839354738379,65.8368832728156,66.8344118072522,67.8319403416887,68.8294688761253,
69.8269974105619,70.4248606341474),.UNSPECIFIED.);
#139=B_SPLINE_CURVE_WITH_KNOTS('',3,(#9190,#9191,#9192,#9193,#9194,#9195,
#9196,#9197,#9198,#9199,#9200,#9201,#9202,#9203,#9204,#9205,#9206,#9207,
#9208,#9209,#9210,#9211),.UNSPECIFIED.,.F.,.F.,(4,3,3,3,3,3,3,4),(-66.6782363354881,
-65.8368832728156,-64.839354738379,-63.8418262039424,-62.8442976695058,
-61.8467691350692,-60.8492406006326,-60.3950510283086),.UNSPECIFIED.);
#140=B_SPLINE_CURVE_WITH_KNOTS('',3,(#9216,#9217,#9218,#9219,#9220,#9221,
#9222,#9223,#9224,#9225,#9226,#9227,#9228,#9229,#9230,#9231,#9232,#9233,
#9234,#9235,#9236,#9237),.UNSPECIFIED.,.F.,.F.,(4,3,3,3,3,3,3,4),(57.8584900197882,
58.8541835317594,59.851712066196,60.8492406006326,61.8467691350692,62.8442976695058,
63.8418262039424,64.1416753269678),.UNSPECIFIED.);
#141=B_SPLINE_CURVE_WITH_KNOTS('',3,(#9238,#9239,#9240,#9241,#9242,#9243,
#9244,#9245,#9246,#9247,#9248,#9249,#9250,#9251,#9252,#9253,#9254,#9255,
#9256,#9257,#9258,#9259),.UNSPECIFIED.,.F.,.F.,(4,3,3,3,3,3,3,4),(-60.3950510283086,
-59.851712066196,-58.8541835317594,-57.8566549973228,-56.8591264628862,
-55.8615979284496,-54.864069394013,-54.111865721129),.UNSPECIFIED.);
#142=B_SPLINE_CURVE_WITH_KNOTS('',3,(#9264,#9265,#9266,#9267,#9268,#9269,
#9270,#9271,#9272,#9273,#9274,#9275,#9276,#9277,#9278,#9279,#9280,#9281,
#9282,#9283,#9284,#9285),.UNSPECIFIED.,.F.,.F.,(4,3,3,3,3,3,3,4),(51.5753047126086,
51.8714837907032,52.8690123251398,53.8665408595764,54.864069394013,55.8615979284496,
56.8591264628862,57.8584900197882),.UNSPECIFIED.);
#143=B_SPLINE_CURVE_WITH_KNOTS('',3,(#9286,#9287,#9288,#9289,#9290,#9291,
#9292,#9293,#9294,#9295,#9296,#9297,#9298,#9299,#9300,#9301,#9302,#9303,
#9304,#9305,#9306,#9307,#9308,#9309,#9310),.UNSPECIFIED.,.F.,.F.,(4,3,3,
3,3,3,3,3,4),(-54.111865721129,-53.8665408595764,-52.8690123251398,-51.8714837907032,
-50.8739552562666,-49.87642672183,-48.8788981873934,-47.8813696529568,-47.8286804139494),
 .UNSPECIFIED.);
#144=B_SPLINE_CURVE_WITH_KNOTS('',3,(#9315,#9316,#9317,#9318,#9319,#9320,
#9321,#9322,#9323,#9324,#9325,#9326,#9327,#9328,#9329,#9330,#9331,#9332,
#9333,#9334,#9335,#9336),.UNSPECIFIED.,.F.,.F.,(4,3,3,3,3,3,3,4),(45.2921194054291,
45.8863125840836,46.8838411185202,47.8813696529568,48.8788981873934,49.87642672183,
50.8739552562666,51.5753047126086),.UNSPECIFIED.);
#145=B_SPLINE_CURVE_WITH_KNOTS('',3,(#9337,#9338,#9339,#9340,#9341,#9342,
#9343,#9344,#9345,#9346,#9347,#9348,#9349,#9350,#9351,#9352,#9353,#9354,
#9355,#9356,#9357,#9358),.UNSPECIFIED.,.F.,.F.,(4,3,3,3,3,3,3,4),(-47.8286804139494,
-46.8838411185202,-45.8863125840836,-44.888784049647,-43.8912555152104,
-42.8937269807738,-41.8961984463372,-41.5454951067698),.UNSPECIFIED.);
#146=B_SPLINE_CURVE_WITH_KNOTS('',3,(#9363,#9364,#9365,#9366,#9367,#9368,
#9369,#9370,#9371,#9372,#9373,#9374,#9375,#9376,#9377,#9378,#9379,#9380,
#9381,#9382,#9383,#9384),.UNSPECIFIED.,.F.,.F.,(4,3,3,3,3,3,3,4),(39.0089340982495,
39.901141377464,40.8986699119006,41.8961984463372,42.8937269807738,43.8912555152104,
44.888784049647,45.2921194054291),.UNSPECIFIED.);
#147=B_SPLINE_CURVE_WITH_KNOTS('',3,(#9385,#9386,#9387,#9388,#9389,#9390,
#9391,#9392,#9393,#9394,#9395,#9396,#9397,#9398,#9399,#9400,#9401,#9402,
#9403,#9404,#9405,#9406),.UNSPECIFIED.,.F.,.F.,(4,3,3,3,3,3,3,4),(-41.5454951067698,
-40.8986699119006,-39.901141377464,-38.9036128430274,-37.9060843085908,
-36.9085557741542,-35.9110272397176,-35.2623097995902),.UNSPECIFIED.);
#148=B_SPLINE_CURVE_WITH_KNOTS('',3,(#9411,#9412,#9413,#9414,#9415,#9416,
#9417,#9418,#9419,#9420,#9421,#9422,#9423,#9424,#9425,#9426,#9427,#9428,
#9429,#9430,#9431,#9432,#9433,#9434,#9435),.UNSPECIFIED.,.F.,.F.,(4,3,3,
3,3,3,3,3,4),(32.7257487910699,32.9184416364078,33.9159701708444,34.913498705281,
35.9110272397176,36.9085557741542,37.9060843085908,38.9036128430274,39.0089340982495),
 .UNSPECIFIED.);
#149=B_SPLINE_CURVE_WITH_KNOTS('',3,(#9436,#9437,#9438,#9439,#9440,#9441,
#9442,#9443,#9444,#9445,#9446,#9447,#9448,#9449,#9450,#9451,#9452,#9453,
#9454,#9455,#9456,#9457),.UNSPECIFIED.,.F.,.F.,(4,3,3,3,3,3,3,4),(-35.2623097995902,
-34.913498705281,-33.9159701708444,-32.9184416364078,-31.9209131019712,
-30.9233845675346,-29.925856033098,-28.9791244924106),.UNSPECIFIED.);
#150=B_SPLINE_CURVE_WITH_KNOTS('',3,(#9462,#9463,#9464,#9465,#9466,#9467,
#9468,#9469,#9470,#9471,#9472,#9473,#9474,#9475,#9476,#9477,#9478,#9479,
#9480,#9481,#9482,#9483),.UNSPECIFIED.,.F.,.F.,(4,3,3,3,3,3,3,4),(26.4425634838903,
26.9332704297882,27.9307989642248,28.9283274986614,29.925856033098,30.9233845675346,
31.9209131019712,32.7257487910699),.UNSPECIFIED.);
#151=B_SPLINE_CURVE_WITH_KNOTS('',3,(#9484,#9485,#9486,#9487,#9488,#9489,
#9490,#9491,#9492,#9493,#9494,#9495,#9496,#9497,#9498,#9499,#9500,#9501,
#9502,#9503,#9504,#9505,#9506,#9507,#9508),.UNSPECIFIED.,.F.,.F.,(4,3,3,
3,3,3,3,3,4),(-28.9791244924106,-28.9283274986614,-27.9307989642248,-26.9332704297882,
-25.9357418953516,-24.938213360915,-23.9406848264784,-22.9431562920418,
-22.695939185231),.UNSPECIFIED.);
#152=B_SPLINE_CURVE_WITH_KNOTS('',3,(#9513,#9514,#9515,#9516,#9517,#9518,
#9519,#9520,#9521,#9522,#9523,#9524,#9525,#9526,#9527,#9528,#9529,#9530,
#9531,#9532,#9533,#9534),.UNSPECIFIED.,.F.,.F.,(4,3,3,3,3,3,3,4),(20.1593781767107,
20.9480992231686,21.9456277576052,22.9431562920418,23.9406848264784,24.938213360915,
25.9357418953516,26.4425634838903),.UNSPECIFIED.);
#153=B_SPLINE_CURVE_WITH_KNOTS('',3,(#9535,#9536,#9537,#9538,#9539,#9540,
#9541,#9542,#9543,#9544,#9545,#9546,#9547,#9548,#9549,#9550,#9551,#9552,
#9553,#9554,#9555,#9556),.UNSPECIFIED.,.F.,.F.,(4,3,3,3,3,3,3,4),(-22.695939185231,
-21.9456277576052,-20.9480992231686,-19.950570688732,-18.9530421542954,
-17.9555136198588,-16.9579850854222,-16.4127538780514),.UNSPECIFIED.);
#154=B_SPLINE_CURVE_WITH_KNOTS('',3,(#9561,#9562,#9563,#9564,#9565,#9566,
#9567,#9568,#9569,#9570,#9571,#9572,#9573,#9574,#9575,#9576,#9577,#9578,
#9579,#9580,#9581,#9582,#9583,#9584,#9585),.UNSPECIFIED.,.F.,.F.,(4,3,3,
3,3,3,3,3,4),(13.8761928695311,13.9653994821124,14.962928016549,15.9604565509856,
16.9579850854222,17.9555136198588,18.9530421542954,19.950570688732,20.1593781767107),
 .UNSPECIFIED.);
#155=B_SPLINE_CURVE_WITH_KNOTS('',3,(#9586,#9587,#9588,#9589,#9590,#9591,
#9592,#9593,#9594,#9595,#9596,#9597,#9598,#9599,#9600,#9601,#9602,#9603,
#9604,#9605,#9606,#9607),.UNSPECIFIED.,.F.,.F.,(4,3,3,3,3,3,3,4),(-16.4127538780514,
-15.9604565509856,-14.962928016549,-13.9653994821124,-12.9678709476758,
-11.9703424132392,-10.9728138788026,-10.1295685708718),.UNSPECIFIED.);
#156=B_SPLINE_CURVE_WITH_KNOTS('',3,(#9613,#9614,#9615,#9616,#9617,#9618,
#9619,#9620,#9621,#9622,#9623,#9624,#9625),.UNSPECIFIED.,.F.,.F.,(4,3,3,
3,4),(-3.84638326369226,-2.9925856033098,-1.9950570688732,-0.997528534436599,
0.),.UNSPECIFIED.);
#157=B_SPLINE_CURVE_WITH_KNOTS('',3,(#9628,#9629,#9630,#9631,#9632,#9633,
#9634,#9635,#9636,#9637,#9638,#9639,#9640,#9641,#9642,#9643,#9644,#9645,
#9646),.UNSPECIFIED.,.F.,.F.,(4,3,3,3,3,3,4),(2.01461286527441,2.99258560330979,
3.99011413774639,4.98764267218299,5.9851712066196,6.98269974105619,7.59300756235152),
 .UNSPECIFIED.);
#158=B_SPLINE_CURVE_WITH_KNOTS('',3,(#9652,#9653,#9654,#9655,#9656,#9657),
 .UNSPECIFIED.,.F.,.F.,(4,1,1,4),(109.955742875643,110.61690491348,111.614433447917,
112.611961982353),.UNSPECIFIED.);
#159=B_SPLINE_CURVE_WITH_KNOTS('',3,(#9660,#9661,#9662,#9663,#9664,#9665,
#9666),.UNSPECIFIED.,.F.,.F.,(4,1,1,1,4),(109.955742875643,110.16088031869,
111.158408853127,112.155937387564,113.133910125599),.UNSPECIFIED.);
#160=B_SPLINE_CURVE_WITH_KNOTS('',3,(#9671,#9672,#9673,#9674,#9675,#9676,
#9677,#9678,#9679,#9680),.UNSPECIFIED.,.F.,.F.,(4,1,1,1,1,1,1,4),(103.672557568463,
104.63173370686,105.629262241297,106.626790775734,107.62431931017,108.621847844607,
109.619376379043,109.955742875643),.UNSPECIFIED.);
#161=B_SPLINE_CURVE_WITH_KNOTS('',3,(#9681,#9682,#9683,#9684,#9685,#9686,
#9687,#9688,#9689,#9690),.UNSPECIFIED.,.F.,.F.,(4,1,1,1,1,1,1,4),(103.672557568463,
104.175709112071,105.173237646507,106.170766180944,107.168294715381,108.165823249817,
109.163351784254,109.955742875643),.UNSPECIFIED.);
#162=B_SPLINE_CURVE_WITH_KNOTS('',3,(#9695,#9696,#9697,#9698,#9699,#9700,
#9701,#9702,#9703,#9704,#9705),.UNSPECIFIED.,.F.,.F.,(4,1,1,1,1,1,1,1,4),
(97.3893722612836,97.6490339658042,98.6465625002408,99.6440910346774,100.641619569114,
101.639148103551,102.636676637987,103.634205172424,103.672557568463),
 .UNSPECIFIED.);
#163=B_SPLINE_CURVE_WITH_KNOTS('',3,(#9706,#9707,#9708,#9709,#9710,#9711,
#9712,#9713,#9714,#9715),.UNSPECIFIED.,.F.,.F.,(4,1,1,1,1,1,1,4),(97.3893722612836,
98.1905379054512,99.1880664398878,100.185594974324,101.183123508761,102.180652043198,
103.178180577634,103.672557568463),.UNSPECIFIED.);
#164=B_SPLINE_CURVE_WITH_KNOTS('',3,(#9720,#9721,#9722,#9723,#9724,#9725,
#9726,#9727,#9728,#9729),.UNSPECIFIED.,.F.,.F.,(4,1,1,1,1,1,1,4),(91.106186954104,
91.6638627591846,92.6613912936212,93.6589198280578,94.6564483624944,95.653976896931,
96.6515054313676,97.3893722612836),.UNSPECIFIED.);
#165=B_SPLINE_CURVE_WITH_KNOTS('',3,(#9730,#9731,#9732,#9733,#9734,#9735,
#9736,#9737,#9738,#9739,#9740),.UNSPECIFIED.,.F.,.F.,(4,1,1,1,1,1,1,1,4),
(91.106186954104,91.207838164395,92.2053666988316,93.2028952332682,94.2004237677048,
95.1979523021414,96.195480836578,97.1930093710146,97.3893722612836),
 .UNSPECIFIED.);
#166=B_SPLINE_CURVE_WITH_KNOTS('',3,(#9745,#9746,#9747,#9748,#9749,#9750,
#9751,#9752,#9753,#9754),.UNSPECIFIED.,.F.,.F.,(4,1,1,1,1,1,1,4),(84.8230016469244,
85.678691552565,86.6762200870016,87.6737486214382,88.6712771558748,89.6688056903114,
90.666334224748,91.106186954104),.UNSPECIFIED.);
#167=B_SPLINE_CURVE_WITH_KNOTS('',3,(#9755,#9756,#9757,#9758,#9759,#9760,
#9761,#9762,#9763,#9764),.UNSPECIFIED.,.F.,.F.,(4,1,1,1,1,1,1,4),(84.8230016469244,
85.2226669577754,86.220195492212,87.2177240266486,88.2152525610852,89.2127810955218,
90.2103096299584,91.106186954104),.UNSPECIFIED.);
#168=B_SPLINE_CURVE_WITH_KNOTS('',3,(#9769,#9770,#9771,#9772,#9773,#9774,
#9775,#9776,#9777,#9778,#9779),.UNSPECIFIED.,.F.,.F.,(4,1,1,1,1,1,1,1,4),
(78.5398163397448,78.6959918115088,79.6935203459454,80.691048880382,81.6885774148186,
82.6861059492552,83.6836344836918,84.6811630181284,84.8230016469244),
 .UNSPECIFIED.);
#169=B_SPLINE_CURVE_WITH_KNOTS('',3,(#9780,#9781,#9782,#9783,#9784,#9785,
#9786,#9787,#9788,#9789),.UNSPECIFIED.,.F.,.F.,(4,1,1,1,1,1,1,4),(78.5398163397448,
79.2374957511558,80.2350242855924,81.232552820029,82.2300813544656,83.2276098889022,
84.2251384233388,84.8230016469244),.UNSPECIFIED.);
#170=B_SPLINE_CURVE_WITH_KNOTS('',3,(#9794,#9795,#9796,#9797,#9798,#9799,
#9800,#9801,#9802,#9803),.UNSPECIFIED.,.F.,.F.,(4,1,1,1,1,1,1,4),(72.2566310325652,
72.7108206048892,73.7083491393258,74.7058776737624,75.703406208199,76.7009347426356,
77.6984632770722,78.5398163397448),.UNSPECIFIED.);
#171=B_SPLINE_CURVE_WITH_KNOTS('',3,(#9804,#9805,#9806,#9807,#9808,#9809,
#9810,#9811,#9812,#9813),.UNSPECIFIED.,.F.,.F.,(4,1,1,1,1,1,1,4),(72.2566310325652,
73.2523245445362,74.2498530789728,75.2473816134094,76.244910147846,77.2424386822826,
78.2399672167192,78.5398163397448),.UNSPECIFIED.);
#172=B_SPLINE_CURVE_WITH_KNOTS('',3,(#9818,#9819,#9820,#9821,#9822,#9823,
#9824,#9825,#9826,#9827),.UNSPECIFIED.,.F.,.F.,(4,1,1,1,1,1,1,4),(65.9734457253856,
66.7256493982696,67.7231779327062,68.7207064671428,69.7182350015794,70.715763536016,
71.7132920704526,72.2566310325652),.UNSPECIFIED.);
#173=B_SPLINE_CURVE_WITH_KNOTS('',3,(#9828,#9829,#9830,#9831,#9832,#9833,
#9834,#9835,#9836,#9837,#9838),.UNSPECIFIED.,.F.,.F.,(4,1,1,1,1,1,1,1,4),
(65.9734457253856,66.26962480348,67.2671533379167,68.2646818723532,69.2622104067898,
70.2597389412264,71.257267475663,72.2547960100996,72.2566310325652),
 .UNSPECIFIED.);
#174=B_SPLINE_CURVE_WITH_KNOTS('',3,(#9843,#9844,#9845,#9846,#9847,#9848,
#9849,#9850,#9851,#9852,#9853),.UNSPECIFIED.,.F.,.F.,(4,1,1,1,1,1,1,1,4),
(59.690260418206,59.7429496572134,60.74047819165,61.7380067260866,62.7355352605232,
63.7330637949598,64.7305923293964,65.728120863833,65.9734457253856),
 .UNSPECIFIED.);
#175=B_SPLINE_CURVE_WITH_KNOTS('',3,(#9854,#9855,#9856,#9857,#9858,#9859,
#9860,#9861,#9862,#9863),.UNSPECIFIED.,.F.,.F.,(4,1,1,1,1,1,1,4),(59.690260418206,
60.2844535968605,61.281982131297,62.2795106657336,63.2770392001703,64.2745677346068,
65.2720962690434,65.9734457253856),.UNSPECIFIED.);
#176=B_SPLINE_CURVE_WITH_KNOTS('',3,(#9868,#9869,#9870,#9871,#9872,#9873,
#9874,#9875,#9876,#9877),.UNSPECIFIED.,.F.,.F.,(4,1,1,1,1,1,1,4),(53.4070751110264,
53.7577784505938,54.7553069850304,55.752835519467,56.7503640539036,57.7478925883402,
58.7454211227768,59.690260418206),.UNSPECIFIED.);
#177=B_SPLINE_CURVE_WITH_KNOTS('',3,(#9878,#9879,#9880,#9881,#9882,#9883,
#9884,#9885,#9886,#9887),.UNSPECIFIED.,.F.,.F.,(4,1,1,1,1,1,1,4),(53.4070751110264,
54.2992823902409,55.2968109246775,56.294339459114,57.2918679935507,58.2893965279873,
59.2869250624238,59.690260418206),.UNSPECIFIED.);
#178=B_SPLINE_CURVE_WITH_KNOTS('',3,(#9892,#9893,#9894,#9895,#9896,#9897,
#9898,#9899,#9900,#9901),.UNSPECIFIED.,.F.,.F.,(4,1,1,1,1,1,1,4),(47.1238898038468,
47.7726072439742,48.7701357784108,49.7676643128474,50.765192847284,51.7627213817206,
52.7602499161572,53.4070751110264),.UNSPECIFIED.);
#179=B_SPLINE_CURVE_WITH_KNOTS('',3,(#9902,#9903,#9904,#9905,#9906,#9907,
#9908,#9909,#9910,#9911,#9912),.UNSPECIFIED.,.F.,.F.,(4,1,1,1,1,1,1,1,4),
(47.1238898038468,47.3165826491847,48.3141111836213,49.3116397180579,50.3091682524945,
51.3066967869311,52.3042253213677,53.3017538558043,53.4070751110264),
 .UNSPECIFIED.);
#180=B_SPLINE_CURVE_WITH_KNOTS('',3,(#9917,#9918,#9919,#9920,#9921,#9922,
#9923,#9924,#9925,#9926),.UNSPECIFIED.,.F.,.F.,(4,1,1,1,1,1,1,4),(40.8407044966673,
41.7874360373546,42.7849645717912,43.7824931062278,44.7800216406644,45.777550175101,
46.7750787095376,47.1238898038468),.UNSPECIFIED.);
#181=B_SPLINE_CURVE_WITH_KNOTS('',3,(#9927,#9928,#9929,#9930,#9931,#9932,
#9933,#9934,#9935,#9936),.UNSPECIFIED.,.F.,.F.,(4,1,1,1,1,1,1,4),(40.8407044966672,
41.3314114425651,42.3289399770017,43.3264685114383,44.3239970458749,45.3215255803115,
46.3190541147481,47.1238898038468),.UNSPECIFIED.);
#182=B_SPLINE_CURVE_WITH_KNOTS('',3,(#9941,#9942,#9943,#9944,#9945,#9946,
#9947,#9948,#9949,#9950,#9951),.UNSPECIFIED.,.F.,.F.,(4,1,1,1,1,1,1,1,4),
(34.5575191894876,34.8047362962984,35.802264830735,36.7997933651716,37.7973218996082,
38.7948504340448,39.7923789684814,40.789907502918,40.8407044966673),
 .UNSPECIFIED.);
#183=B_SPLINE_CURVE_WITH_KNOTS('',3,(#9952,#9953,#9954,#9955,#9956,#9957,
#9958,#9959,#9960,#9961),.UNSPECIFIED.,.F.,.F.,(4,1,1,1,1,1,1,4),(34.5575191894876,
35.3462402359455,36.3437687703821,37.3412973048187,38.3388258392553,39.3363543736919,
40.3338829081285,40.8407044966672),.UNSPECIFIED.);
#184=B_SPLINE_CURVE_WITH_KNOTS('',3,(#9966,#9967,#9968,#9969,#9970,#9971,
#9972,#9973,#9974,#9975),.UNSPECIFIED.,.F.,.F.,(4,1,1,1,1,1,1,4),(28.2743338823081,
28.8195650896788,29.8170936241154,30.814622158552,31.8121506929886,32.8096792274252,
33.8072077618618,34.5575191894876),.UNSPECIFIED.);
#185=B_SPLINE_CURVE_WITH_KNOTS('',3,(#9976,#9977,#9978,#9979,#9980,#9981,
#9982,#9983,#9984,#9985,#9986),.UNSPECIFIED.,.F.,.F.,(4,1,1,1,1,1,1,1,4),
(28.274333882308,28.3635404948893,29.3610690293259,30.3585975637625,31.3561260981991,
32.3536546326357,33.3511831670723,34.3487117015089,34.5575191894876),
 .UNSPECIFIED.);
#186=B_SPLINE_CURVE_WITH_KNOTS('',3,(#9991,#9992,#9993,#9994,#9995,#9996,
#9997,#9998,#9999,#10000),.UNSPECIFIED.,.F.,.F.,(4,1,1,1,1,1,1,4),(21.9911485751285,
22.8343938830592,23.8319224174958,24.8294509519324,25.826979486369,26.8245080208056,
27.8220365552422,28.2743338823081),.UNSPECIFIED.);
#187=B_SPLINE_CURVE_WITH_KNOTS('',3,(#10001,#10002,#10003,#10004,#10005,
#10006,#10007,#10008,#10009,#10010),.UNSPECIFIED.,.F.,.F.,(4,1,1,1,1,1,
1,4),(21.9911485751285,22.3783692882697,23.3758978227063,24.3734263571429,
25.3709548915795,26.3684834260161,27.3660119604527,28.274333882308),
 .UNSPECIFIED.);
#188=B_SPLINE_CURVE_WITH_KNOTS('',3,(#10016,#10017,#10018,#10019,#10020),
 .UNSPECIFIED.,.F.,.F.,(4,1,4),(14.3981410127769,15.3956695472135,15.7079632679489),
 .UNSPECIFIED.);
#189=B_SPLINE_CURVE_WITH_KNOTS('',3,(#10023,#10024,#10025,#10026,#10027),
 .UNSPECIFIED.,.F.,.F.,(4,1,4),(13.8761928695311,14.8541656075664,15.7079632679489),
 .UNSPECIFIED.);
#190=B_SPLINE_CURVE_WITH_KNOTS('',3,(#10033,#10034,#10035,#10036,#10037,
#10038,#10039,#10040,#10041,#10042,#10043,#10044,#10045,#10046,#10047,#10048,
#10049,#10050,#10051),.UNSPECIFIED.,.F.,.F.,(4,3,3,3,3,3,4),(95.5576018628658,
95.7627393059135,96.7602678403501,97.7577963747867,98.7553249092233,99.7528534436599,
100.750381978097),.UNSPECIFIED.);
#191=B_SPLINE_CURVE_WITH_KNOTS('',3,(#10055,#10056,#10057,#10058),
 .UNSPECIFIED.,.F.,.F.,(4,4),(-98.7357691128221,-98.0941628713861),
 .UNSPECIFIED.);
#192=B_SPLINE_CURVE_WITH_KNOTS('',3,(#10062,#10063,#10064,#10065,#10066,
#10067,#10068,#10069,#10070,#10071,#10072,#10073,#10074,#10075,#10076,#10077,
#10078,#10079,#10080,#10081,#10082,#10083),.UNSPECIFIED.,.F.,.F.,(4,3,3,
3,3,3,3,4),(-98.0941628713861,-97.7577963747867,-96.7602678403501,-95.7627393059135,
-94.7652107714769,-93.7676822370403,-92.7701537026037,-91.8109775642065),
 .UNSPECIFIED.);
#193=B_SPLINE_CURVE_WITH_KNOTS('',3,(#10088,#10089,#10090,#10091,#10092,
#10093,#10094,#10095,#10096,#10097,#10098,#10099,#10100,#10101,#10102,#10103,
#10104,#10105,#10106,#10107,#10108,#10109),.UNSPECIFIED.,.F.,.F.,(4,3,3,
3,3,3,3,4),(89.2744165556862,89.7775680992939,90.7750966337306,91.7726251681671,
92.7701537026037,93.7676822370403,94.7652107714769,95.5576018628658),
 .UNSPECIFIED.);
#194=B_SPLINE_CURVE_WITH_KNOTS('',3,(#10110,#10111,#10112,#10113,#10114,
#10115,#10116,#10117,#10118,#10119,#10120,#10121,#10122,#10123,#10124,#10125,
#10126,#10127,#10128,#10129,#10130,#10131,#10132,#10133,#10134),
 .UNSPECIFIED.,.F.,.F.,(4,3,3,3,3,3,3,3,4),(-91.8109775642065,-91.7726251681671,
-90.7750966337305,-89.7775680992939,-88.7800395648573,-87.7825110304207,
-86.7849824959842,-85.7874539615476,-85.5277922570269),.UNSPECIFIED.);
#195=B_SPLINE_CURVE_WITH_KNOTS('',3,(#10139,#10140,#10141,#10142,#10143,
#10144,#10145,#10146,#10147,#10148,#10149,#10150,#10151,#10152,#10153,#10154,
#10155,#10156,#10157,#10158,#10159,#10160),.UNSPECIFIED.,.F.,.F.,(4,3,3,
3,3,3,3,4),(82.9912312485066,83.7923968926743,84.7899254271109,85.7874539615476,
86.7849824959841,87.7825110304207,88.7800395648573,89.2744165556862),
 .UNSPECIFIED.);
#196=B_SPLINE_CURVE_WITH_KNOTS('',3,(#10161,#10162,#10163,#10164,#10165,
#10166,#10167,#10168,#10169,#10170,#10171,#10172,#10173,#10174,#10175,#10176,
#10177,#10178,#10179,#10180,#10181,#10182),.UNSPECIFIED.,.F.,.F.,(4,3,3,
3,3,3,3,4),(-85.5277922570269,-84.789925427111,-83.7923968926743,-82.7948683582377,
-81.7973398238011,-80.7998112893646,-79.8022827549279,-79.2446069498473),
 .UNSPECIFIED.);
#197=B_SPLINE_CURVE_WITH_KNOTS('',3,(#10187,#10188,#10189,#10190,#10191,
#10192,#10193,#10194,#10195,#10196,#10197,#10198,#10199,#10200,#10201,#10202,
#10203,#10204,#10205,#10206,#10207,#10208,#10209,#10210,#10211),
 .UNSPECIFIED.,.F.,.F.,(4,3,3,3,3,3,3,3,4),(76.708045941327,76.8096971516181,
77.8072256860547,78.8047542204914,79.8022827549279,80.7998112893646,81.7973398238011,
82.7948683582377,82.9912312485066),.UNSPECIFIED.);
#198=B_SPLINE_CURVE_WITH_KNOTS('',3,(#10212,#10213,#10214,#10215,#10216,
#10217,#10218,#10219,#10220,#10221,#10222,#10223,#10224,#10225,#10226,#10227,
#10228,#10229,#10230,#10231,#10232,#10233),.UNSPECIFIED.,.F.,.F.,(4,3,3,
3,3,3,3,4),(-79.2446069498473,-78.8047542204913,-77.8072256860547,-76.8096971516181,
-75.8121686171815,-74.8146400827449,-73.8171115483083,-72.9614216426677),
 .UNSPECIFIED.);
#199=B_SPLINE_CURVE_WITH_KNOTS('',3,(#10238,#10239,#10240,#10241,#10242,
#10243,#10244,#10245,#10246,#10247,#10248,#10249,#10250,#10251,#10252,#10253,
#10254,#10255,#10256,#10257,#10258,#10259),.UNSPECIFIED.,.F.,.F.,(4,3,3,
3,3,3,3,4),(70.4248606341474,70.8245259449985,71.8220544794352,72.8195830138717,
73.8171115483084,74.8146400827449,75.8121686171816,76.708045941327),
 .UNSPECIFIED.);
#200=B_SPLINE_CURVE_WITH_KNOTS('',3,(#10260,#10261,#10262,#10263,#10264,
#10265,#10266,#10267,#10268,#10269,#10270,#10271,#10272,#10273,#10274,#10275,
#10276,#10277,#10278,#10279,#10280,#10281,#10282,#10283,#10284),
 .UNSPECIFIED.,.F.,.F.,(4,3,3,3,3,3,3,3,4),(-72.9614216426677,-72.8195830138717,
-71.8220544794352,-70.8245259449986,-69.8269974105619,-68.8294688761253,
-67.8319403416887,-66.8344118072522,-66.6782363354881),.UNSPECIFIED.);
#201=B_SPLINE_CURVE_WITH_KNOTS('',3,(#10289,#10290,#10291,#10292,#10293,
#10294,#10295,#10296,#10297,#10298,#10299,#10300,#10301,#10302,#10303,#10304,
#10305,#10306,#10307,#10308,#10309,#10310),.UNSPECIFIED.,.F.,.F.,(4,3,3,
3,3,3,3,4),(64.1416753269678,64.839354738379,65.8368832728156,66.8344118072522,
67.8319403416887,68.8294688761253,69.8269974105619,70.4248606341474),
 .UNSPECIFIED.);
#202=B_SPLINE_CURVE_WITH_KNOTS('',3,(#10311,#10312,#10313,#10314,#10315,
#10316,#10317,#10318,#10319,#10320,#10321,#10322,#10323,#10324,#10325,#10326,
#10327,#10328,#10329,#10330,#10331,#10332),.UNSPECIFIED.,.F.,.F.,(4,3,3,
3,3,3,3,4),(-66.6782363354881,-65.8368832728156,-64.839354738379,-63.8418262039424,
-62.8442976695058,-61.8467691350692,-60.8492406006326,-60.3950510283086),
 .UNSPECIFIED.);
#203=B_SPLINE_CURVE_WITH_KNOTS('',3,(#10337,#10338,#10339,#10340,#10341,
#10342,#10343,#10344,#10345,#10346,#10347,#10348,#10349,#10350,#10351,#10352,
#10353,#10354,#10355,#10356,#10357,#10358),.UNSPECIFIED.,.F.,.F.,(4,3,3,
3,3,3,3,4),(57.8584900197882,58.8541835317594,59.851712066196,60.8492406006326,
61.8467691350692,62.8442976695058,63.8418262039424,64.1416753269678),
 .UNSPECIFIED.);
#204=B_SPLINE_CURVE_WITH_KNOTS('',3,(#10359,#10360,#10361,#10362,#10363,
#10364,#10365,#10366,#10367,#10368,#10369,#10370,#10371,#10372,#10373,#10374,
#10375,#10376,#10377,#10378,#10379,#10380),.UNSPECIFIED.,.F.,.F.,(4,3,3,
3,3,3,3,4),(-60.3950510283086,-59.851712066196,-58.8541835317594,-57.8566549973228,
-56.8591264628862,-55.8615979284496,-54.864069394013,-54.111865721129),
 .UNSPECIFIED.);
#205=B_SPLINE_CURVE_WITH_KNOTS('',3,(#10385,#10386,#10387,#10388,#10389,
#10390,#10391,#10392,#10393,#10394,#10395,#10396,#10397,#10398,#10399,#10400,
#10401,#10402,#10403,#10404,#10405,#10406),.UNSPECIFIED.,.F.,.F.,(4,3,3,
3,3,3,3,4),(51.5753047126086,51.8714837907032,52.8690123251398,53.8665408595764,
54.864069394013,55.8615979284496,56.8591264628862,57.8584900197882),
 .UNSPECIFIED.);
#206=B_SPLINE_CURVE_WITH_KNOTS('',3,(#10407,#10408,#10409,#10410,#10411,
#10412,#10413,#10414,#10415,#10416,#10417,#10418,#10419,#10420,#10421,#10422,
#10423,#10424,#10425,#10426,#10427,#10428,#10429,#10430,#10431),
 .UNSPECIFIED.,.F.,.F.,(4,3,3,3,3,3,3,3,4),(-54.111865721129,-53.8665408595764,
-52.8690123251398,-51.8714837907032,-50.8739552562666,-49.87642672183,-48.8788981873934,
-47.8813696529568,-47.8286804139494),.UNSPECIFIED.);
#207=B_SPLINE_CURVE_WITH_KNOTS('',3,(#10436,#10437,#10438,#10439,#10440,
#10441,#10442,#10443,#10444,#10445,#10446,#10447,#10448,#10449,#10450,#10451,
#10452,#10453,#10454,#10455,#10456,#10457),.UNSPECIFIED.,.F.,.F.,(4,3,3,
3,3,3,3,4),(45.2921194054291,45.8863125840836,46.8838411185202,47.8813696529568,
48.8788981873934,49.87642672183,50.8739552562666,51.5753047126086),
 .UNSPECIFIED.);
#208=B_SPLINE_CURVE_WITH_KNOTS('',3,(#10458,#10459,#10460,#10461,#10462,
#10463,#10464,#10465,#10466,#10467,#10468,#10469,#10470,#10471,#10472,#10473,
#10474,#10475,#10476,#10477,#10478,#10479),.UNSPECIFIED.,.F.,.F.,(4,3,3,
3,3,3,3,4),(-47.8286804139494,-46.8838411185202,-45.8863125840836,-44.888784049647,
-43.8912555152104,-42.8937269807738,-41.8961984463372,-41.5454951067698),
 .UNSPECIFIED.);
#209=B_SPLINE_CURVE_WITH_KNOTS('',3,(#10484,#10485,#10486,#10487,#10488,
#10489,#10490,#10491,#10492,#10493,#10494,#10495,#10496,#10497,#10498,#10499,
#10500,#10501,#10502,#10503,#10504,#10505),.UNSPECIFIED.,.F.,.F.,(4,3,3,
3,3,3,3,4),(39.0089340982495,39.901141377464,40.8986699119006,41.8961984463372,
42.8937269807738,43.8912555152104,44.888784049647,45.2921194054291),
 .UNSPECIFIED.);
#210=B_SPLINE_CURVE_WITH_KNOTS('',3,(#10506,#10507,#10508,#10509,#10510,
#10511,#10512,#10513,#10514,#10515,#10516,#10517,#10518,#10519,#10520,#10521,
#10522,#10523,#10524,#10525,#10526,#10527),.UNSPECIFIED.,.F.,.F.,(4,3,3,
3,3,3,3,4),(-41.5454951067698,-40.8986699119006,-39.901141377464,-38.9036128430274,
-37.9060843085908,-36.9085557741542,-35.9110272397176,-35.2623097995902),
 .UNSPECIFIED.);
#211=B_SPLINE_CURVE_WITH_KNOTS('',3,(#10532,#10533,#10534,#10535,#10536,
#10537,#10538,#10539,#10540,#10541,#10542,#10543,#10544,#10545,#10546,#10547,
#10548,#10549,#10550,#10551,#10552,#10553,#10554,#10555,#10556),
 .UNSPECIFIED.,.F.,.F.,(4,3,3,3,3,3,3,3,4),(32.7257487910699,32.9184416364078,
33.9159701708444,34.913498705281,35.9110272397176,36.9085557741542,37.9060843085908,
38.9036128430274,39.0089340982495),.UNSPECIFIED.);
#212=B_SPLINE_CURVE_WITH_KNOTS('',3,(#10557,#10558,#10559,#10560,#10561,
#10562,#10563,#10564,#10565,#10566,#10567,#10568,#10569,#10570,#10571,#10572,
#10573,#10574,#10575,#10576,#10577,#10578),.UNSPECIFIED.,.F.,.F.,(4,3,3,
3,3,3,3,4),(-35.2623097995902,-34.913498705281,-33.9159701708444,-32.9184416364078,
-31.9209131019712,-30.9233845675346,-29.925856033098,-28.9791244924106),
 .UNSPECIFIED.);
#213=B_SPLINE_CURVE_WITH_KNOTS('',3,(#10583,#10584,#10585,#10586,#10587,
#10588,#10589,#10590,#10591,#10592,#10593,#10594,#10595,#10596,#10597,#10598,
#10599,#10600,#10601,#10602,#10603,#10604),.UNSPECIFIED.,.F.,.F.,(4,3,3,
3,3,3,3,4),(26.4425634838903,26.9332704297882,27.9307989642248,28.9283274986614,
29.925856033098,30.9233845675346,31.9209131019712,32.7257487910699),
 .UNSPECIFIED.);
#214=B_SPLINE_CURVE_WITH_KNOTS('',3,(#10605,#10606,#10607,#10608,#10609,
#10610,#10611,#10612,#10613,#10614,#10615,#10616,#10617,#10618,#10619,#10620,
#10621,#10622,#10623,#10624,#10625,#10626,#10627,#10628,#10629),
 .UNSPECIFIED.,.F.,.F.,(4,3,3,3,3,3,3,3,4),(-28.9791244924106,-28.9283274986614,
-27.9307989642248,-26.9332704297882,-25.9357418953516,-24.938213360915,
-23.9406848264784,-22.9431562920418,-22.695939185231),.UNSPECIFIED.);
#215=B_SPLINE_CURVE_WITH_KNOTS('',3,(#10634,#10635,#10636,#10637,#10638,
#10639,#10640,#10641,#10642,#10643,#10644,#10645,#10646,#10647,#10648,#10649,
#10650,#10651,#10652,#10653,#10654,#10655),.UNSPECIFIED.,.F.,.F.,(4,3,3,
3,3,3,3,4),(20.1593781767107,20.9480992231686,21.9456277576052,22.9431562920418,
23.9406848264784,24.938213360915,25.9357418953516,26.4425634838903),
 .UNSPECIFIED.);
#216=B_SPLINE_CURVE_WITH_KNOTS('',3,(#10656,#10657,#10658,#10659,#10660,
#10661,#10662,#10663,#10664,#10665,#10666,#10667,#10668,#10669,#10670,#10671,
#10672,#10673,#10674,#10675,#10676,#10677),.UNSPECIFIED.,.F.,.F.,(4,3,3,
3,3,3,3,4),(-22.695939185231,-21.9456277576052,-20.9480992231686,-19.950570688732,
-18.9530421542954,-17.9555136198588,-16.9579850854222,-16.4127538780514),
 .UNSPECIFIED.);
#217=B_SPLINE_CURVE_WITH_KNOTS('',3,(#10682,#10683,#10684,#10685,#10686,
#10687,#10688,#10689,#10690,#10691,#10692,#10693,#10694,#10695,#10696,#10697,
#10698,#10699,#10700,#10701,#10702,#10703,#10704,#10705,#10706),
 .UNSPECIFIED.,.F.,.F.,(4,3,3,3,3,3,3,3,4),(13.8761928695311,13.9653994821124,
14.962928016549,15.9604565509856,16.9579850854222,17.9555136198588,18.9530421542954,
19.950570688732,20.1593781767107),.UNSPECIFIED.);
#218=B_SPLINE_CURVE_WITH_KNOTS('',3,(#10707,#10708,#10709,#10710,#10711,
#10712,#10713,#10714,#10715,#10716,#10717,#10718,#10719,#10720,#10721,#10722,
#10723,#10724,#10725,#10726,#10727,#10728),.UNSPECIFIED.,.F.,.F.,(4,3,3,
3,3,3,3,4),(-16.4127538780514,-15.9604565509856,-14.962928016549,-13.9653994821124,
-12.9678709476758,-11.9703424132392,-10.9728138788026,-10.1295685708718),
 .UNSPECIFIED.);
#219=B_SPLINE_CURVE_WITH_KNOTS('',3,(#10734,#10735,#10736,#10737,#10738,
#10739,#10740,#10741,#10742,#10743,#10744,#10745,#10746),.UNSPECIFIED.,
 .F.,.F.,(4,3,3,3,4),(-3.84638326369226,-2.9925856033098,-1.9950570688732,
-0.997528534436599,0.),.UNSPECIFIED.);
#220=B_SPLINE_CURVE_WITH_KNOTS('',3,(#10749,#10750,#10751,#10752,#10753,
#10754,#10755,#10756,#10757,#10758,#10759,#10760,#10761,#10762,#10763,#10764,
#10765,#10766,#10767),.UNSPECIFIED.,.F.,.F.,(4,3,3,3,3,3,4),(2.01461286527441,
2.99258560330979,3.99011413774639,4.98764267218299,5.9851712066196,6.98269974105619,
7.59300756235152),.UNSPECIFIED.);
#221=B_SPLINE_CURVE_WITH_KNOTS('',3,(#10773,#10774,#10775,#10776,#10777,
#10778),.UNSPECIFIED.,.F.,.F.,(4,1,1,4),(109.955742875643,110.61690491348,
111.614433447917,112.611961982353),.UNSPECIFIED.);
#222=B_SPLINE_CURVE_WITH_KNOTS('',3,(#10781,#10782,#10783,#10784,#10785,
#10786,#10787),.UNSPECIFIED.,.F.,.F.,(4,1,1,1,4),(109.955742875643,110.16088031869,
111.158408853127,112.155937387564,113.133910125599),.UNSPECIFIED.);
#223=B_SPLINE_CURVE_WITH_KNOTS('',3,(#10792,#10793,#10794,#10795,#10796,
#10797,#10798,#10799,#10800,#10801),.UNSPECIFIED.,.F.,.F.,(4,1,1,1,1,1,
1,4),(103.672557568463,104.63173370686,105.629262241297,106.626790775734,
107.62431931017,108.621847844607,109.619376379043,109.955742875643),
 .UNSPECIFIED.);
#224=B_SPLINE_CURVE_WITH_KNOTS('',3,(#10802,#10803,#10804,#10805,#10806,
#10807,#10808,#10809,#10810,#10811),.UNSPECIFIED.,.F.,.F.,(4,1,1,1,1,1,
1,4),(103.672557568463,104.175709112071,105.173237646507,106.170766180944,
107.168294715381,108.165823249817,109.163351784254,109.955742875643),
 .UNSPECIFIED.);
#225=B_SPLINE_CURVE_WITH_KNOTS('',3,(#10816,#10817,#10818,#10819,#10820,
#10821,#10822,#10823,#10824,#10825,#10826),.UNSPECIFIED.,.F.,.F.,(4,1,1,
1,1,1,1,1,4),(97.3893722612836,97.6490339658042,98.6465625002408,99.6440910346774,
100.641619569114,101.639148103551,102.636676637987,103.634205172424,103.672557568463),
 .UNSPECIFIED.);
#226=B_SPLINE_CURVE_WITH_KNOTS('',3,(#10827,#10828,#10829,#10830,#10831,
#10832,#10833,#10834,#10835,#10836),.UNSPECIFIED.,.F.,.F.,(4,1,1,1,1,1,
1,4),(97.3893722612836,98.1905379054512,99.1880664398878,100.185594974324,
101.183123508761,102.180652043198,103.178180577634,103.672557568463),
 .UNSPECIFIED.);
#227=B_SPLINE_CURVE_WITH_KNOTS('',3,(#10841,#10842,#10843,#10844,#10845,
#10846,#10847,#10848,#10849,#10850),.UNSPECIFIED.,.F.,.F.,(4,1,1,1,1,1,
1,4),(91.106186954104,91.6638627591846,92.6613912936212,93.6589198280578,
94.6564483624944,95.653976896931,96.6515054313676,97.3893722612836),
 .UNSPECIFIED.);
#228=B_SPLINE_CURVE_WITH_KNOTS('',3,(#10851,#10852,#10853,#10854,#10855,
#10856,#10857,#10858,#10859,#10860,#10861),.UNSPECIFIED.,.F.,.F.,(4,1,1,
1,1,1,1,1,4),(91.106186954104,91.207838164395,92.2053666988316,93.2028952332682,
94.2004237677048,95.1979523021414,96.195480836578,97.1930093710146,97.3893722612836),
 .UNSPECIFIED.);
#229=B_SPLINE_CURVE_WITH_KNOTS('',3,(#10866,#10867,#10868,#10869,#10870,
#10871,#10872,#10873,#10874,#10875),.UNSPECIFIED.,.F.,.F.,(4,1,1,1,1,1,
1,4),(84.8230016469244,85.678691552565,86.6762200870016,87.6737486214382,
88.6712771558748,89.6688056903114,90.666334224748,91.106186954104),
 .UNSPECIFIED.);
#230=B_SPLINE_CURVE_WITH_KNOTS('',3,(#10876,#10877,#10878,#10879,#10880,
#10881,#10882,#10883,#10884,#10885),.UNSPECIFIED.,.F.,.F.,(4,1,1,1,1,1,
1,4),(84.8230016469244,85.2226669577754,86.220195492212,87.2177240266486,
88.2152525610852,89.2127810955218,90.2103096299584,91.106186954104),
 .UNSPECIFIED.);
#231=B_SPLINE_CURVE_WITH_KNOTS('',3,(#10890,#10891,#10892,#10893,#10894,
#10895,#10896,#10897,#10898,#10899,#10900),.UNSPECIFIED.,.F.,.F.,(4,1,1,
1,1,1,1,1,4),(78.5398163397448,78.6959918115088,79.6935203459454,80.691048880382,
81.6885774148186,82.6861059492552,83.6836344836918,84.6811630181284,84.8230016469244),
 .UNSPECIFIED.);
#232=B_SPLINE_CURVE_WITH_KNOTS('',3,(#10901,#10902,#10903,#10904,#10905,
#10906,#10907,#10908,#10909,#10910),.UNSPECIFIED.,.F.,.F.,(4,1,1,1,1,1,
1,4),(78.5398163397448,79.2374957511558,80.2350242855924,81.232552820029,
82.2300813544656,83.2276098889022,84.2251384233388,84.8230016469244),
 .UNSPECIFIED.);
#233=B_SPLINE_CURVE_WITH_KNOTS('',3,(#10915,#10916,#10917,#10918,#10919,
#10920,#10921,#10922,#10923,#10924),.UNSPECIFIED.,.F.,.F.,(4,1,1,1,1,1,
1,4),(72.2566310325652,72.7108206048892,73.7083491393258,74.7058776737624,
75.703406208199,76.7009347426356,77.6984632770722,78.5398163397448),
 .UNSPECIFIED.);
#234=B_SPLINE_CURVE_WITH_KNOTS('',3,(#10925,#10926,#10927,#10928,#10929,
#10930,#10931,#10932,#10933,#10934),.UNSPECIFIED.,.F.,.F.,(4,1,1,1,1,1,
1,4),(72.2566310325652,73.2523245445362,74.2498530789728,75.2473816134094,
76.244910147846,77.2424386822826,78.2399672167192,78.5398163397448),
 .UNSPECIFIED.);
#235=B_SPLINE_CURVE_WITH_KNOTS('',3,(#10939,#10940,#10941,#10942,#10943,
#10944,#10945,#10946,#10947,#10948),.UNSPECIFIED.,.F.,.F.,(4,1,1,1,1,1,
1,4),(65.9734457253856,66.7256493982696,67.7231779327062,68.7207064671428,
69.7182350015794,70.715763536016,71.7132920704526,72.2566310325652),
 .UNSPECIFIED.);
#236=B_SPLINE_CURVE_WITH_KNOTS('',3,(#10949,#10950,#10951,#10952,#10953,
#10954,#10955,#10956,#10957,#10958,#10959),.UNSPECIFIED.,.F.,.F.,(4,1,1,
1,1,1,1,1,4),(65.9734457253856,66.26962480348,67.2671533379167,68.2646818723532,
69.2622104067898,70.2597389412264,71.257267475663,72.2547960100996,72.2566310325652),
 .UNSPECIFIED.);
#237=B_SPLINE_CURVE_WITH_KNOTS('',3,(#10964,#10965,#10966,#10967,#10968,
#10969,#10970,#10971,#10972,#10973,#10974),.UNSPECIFIED.,.F.,.F.,(4,1,1,
1,1,1,1,1,4),(59.690260418206,59.7429496572134,60.74047819165,61.7380067260866,
62.7355352605232,63.7330637949598,64.7305923293964,65.728120863833,65.9734457253856),
 .UNSPECIFIED.);
#238=B_SPLINE_CURVE_WITH_KNOTS('',3,(#10975,#10976,#10977,#10978,#10979,
#10980,#10981,#10982,#10983,#10984),.UNSPECIFIED.,.F.,.F.,(4,1,1,1,1,1,
1,4),(59.690260418206,60.2844535968605,61.281982131297,62.2795106657336,
63.2770392001703,64.2745677346068,65.2720962690434,65.9734457253856),
 .UNSPECIFIED.);
#239=B_SPLINE_CURVE_WITH_KNOTS('',3,(#10989,#10990,#10991,#10992,#10993,
#10994,#10995,#10996,#10997,#10998),.UNSPECIFIED.,.F.,.F.,(4,1,1,1,1,1,
1,4),(53.4070751110264,53.7577784505938,54.7553069850304,55.752835519467,
56.7503640539036,57.7478925883402,58.7454211227768,59.690260418206),
 .UNSPECIFIED.);
#240=B_SPLINE_CURVE_WITH_KNOTS('',3,(#10999,#11000,#11001,#11002,#11003,
#11004,#11005,#11006,#11007,#11008),.UNSPECIFIED.,.F.,.F.,(4,1,1,1,1,1,
1,4),(53.4070751110264,54.2992823902409,55.2968109246775,56.294339459114,
57.2918679935507,58.2893965279873,59.2869250624238,59.690260418206),
 .UNSPECIFIED.);
#241=B_SPLINE_CURVE_WITH_KNOTS('',3,(#11013,#11014,#11015,#11016,#11017,
#11018,#11019,#11020,#11021,#11022),.UNSPECIFIED.,.F.,.F.,(4,1,1,1,1,1,
1,4),(47.1238898038468,47.7726072439742,48.7701357784108,49.7676643128474,
50.765192847284,51.7627213817206,52.7602499161572,53.4070751110264),
 .UNSPECIFIED.);
#242=B_SPLINE_CURVE_WITH_KNOTS('',3,(#11023,#11024,#11025,#11026,#11027,
#11028,#11029,#11030,#11031,#11032,#11033),.UNSPECIFIED.,.F.,.F.,(4,1,1,
1,1,1,1,1,4),(47.1238898038468,47.3165826491847,48.3141111836213,49.3116397180579,
50.3091682524945,51.3066967869311,52.3042253213677,53.3017538558043,53.4070751110264),
 .UNSPECIFIED.);
#243=B_SPLINE_CURVE_WITH_KNOTS('',3,(#11038,#11039,#11040,#11041,#11042,
#11043,#11044,#11045,#11046,#11047),.UNSPECIFIED.,.F.,.F.,(4,1,1,1,1,1,
1,4),(40.8407044966673,41.7874360373546,42.7849645717912,43.7824931062278,
44.7800216406644,45.777550175101,46.7750787095376,47.1238898038468),
 .UNSPECIFIED.);
#244=B_SPLINE_CURVE_WITH_KNOTS('',3,(#11048,#11049,#11050,#11051,#11052,
#11053,#11054,#11055,#11056,#11057),.UNSPECIFIED.,.F.,.F.,(4,1,1,1,1,1,
1,4),(40.8407044966672,41.3314114425651,42.3289399770017,43.3264685114383,
44.3239970458749,45.3215255803115,46.3190541147481,47.1238898038468),
 .UNSPECIFIED.);
#245=B_SPLINE_CURVE_WITH_KNOTS('',3,(#11062,#11063,#11064,#11065,#11066,
#11067,#11068,#11069,#11070,#11071,#11072),.UNSPECIFIED.,.F.,.F.,(4,1,1,
1,1,1,1,1,4),(34.5575191894876,34.8047362962984,35.802264830735,36.7997933651716,
37.7973218996082,38.7948504340448,39.7923789684814,40.789907502918,40.8407044966673),
 .UNSPECIFIED.);
#246=B_SPLINE_CURVE_WITH_KNOTS('',3,(#11073,#11074,#11075,#11076,#11077,
#11078,#11079,#11080,#11081,#11082),.UNSPECIFIED.,.F.,.F.,(4,1,1,1,1,1,
1,4),(34.5575191894876,35.3462402359455,36.3437687703821,37.3412973048187,
38.3388258392553,39.3363543736919,40.3338829081285,40.8407044966672),
 .UNSPECIFIED.);
#247=B_SPLINE_CURVE_WITH_KNOTS('',3,(#11087,#11088,#11089,#11090,#11091,
#11092,#11093,#11094,#11095,#11096),.UNSPECIFIED.,.F.,.F.,(4,1,1,1,1,1,
1,4),(28.2743338823081,28.8195650896788,29.8170936241154,30.814622158552,
31.8121506929886,32.8096792274252,33.8072077618618,34.5575191894876),
 .UNSPECIFIED.);
#248=B_SPLINE_CURVE_WITH_KNOTS('',3,(#11097,#11098,#11099,#11100,#11101,
#11102,#11103,#11104,#11105,#11106,#11107),.UNSPECIFIED.,.F.,.F.,(4,1,1,
1,1,1,1,1,4),(28.274333882308,28.3635404948893,29.3610690293259,30.3585975637625,
31.3561260981991,32.3536546326357,33.3511831670723,34.3487117015089,34.5575191894876),
 .UNSPECIFIED.);
#249=B_SPLINE_CURVE_WITH_KNOTS('',3,(#11112,#11113,#11114,#11115,#11116,
#11117,#11118,#11119,#11120,#11121),.UNSPECIFIED.,.F.,.F.,(4,1,1,1,1,1,
1,4),(21.9911485751285,22.8343938830592,23.8319224174958,24.8294509519324,
25.826979486369,26.8245080208056,27.8220365552422,28.2743338823081),
 .UNSPECIFIED.);
#250=B_SPLINE_CURVE_WITH_KNOTS('',3,(#11122,#11123,#11124,#11125,#11126,
#11127,#11128,#11129,#11130,#11131),.UNSPECIFIED.,.F.,.F.,(4,1,1,1,1,1,
1,4),(21.9911485751285,22.3783692882697,23.3758978227063,24.3734263571429,
25.3709548915795,26.3684834260161,27.3660119604527,28.274333882308),
 .UNSPECIFIED.);
#251=B_SPLINE_CURVE_WITH_KNOTS('',3,(#11137,#11138,#11139,#11140,#11141),
 .UNSPECIFIED.,.F.,.F.,(4,1,4),(14.3981410127769,15.3956695472135,15.7079632679489),
 .UNSPECIFIED.);
#252=B_SPLINE_CURVE_WITH_KNOTS('',3,(#11144,#11145,#11146,#11147,#11148),
 .UNSPECIFIED.,.F.,.F.,(4,1,4),(13.8761928695311,14.8541656075664,15.7079632679489),
 .UNSPECIFIED.);
#253=B_SPLINE_CURVE_WITH_KNOTS('',3,(#11150,#11151,#11152,#11153,#11154,
#11155,#11156,#11157,#11158,#11159,#11160,#11161,#11162,#11163,#11164,#11165,
#11166,#11167,#11168,#11169,#11170,#11171,#11172,#11173,#11174,#11175,#11176,
#11177,#11178,#11179,#11180,#11181,#11182,#11183,#11184,#11185,#11186,#11187,
#11188,#11189,#11190,#11191,#11192,#11193,#11194,#11195,#11196,#11197,#11198,
#11199,#11200,#11201,#11202,#11203,#11204,#11205,#11206,#11207,#11208,#11209,
#11210,#11211,#11212,#11213,#11214,#11215,#11216,#11217,#11218,#11219,#11220,
#11221,#11222,#11223,#11224,#11225,#11226,#11227,#11228,#11229,#11230,#11231,
#11232,#11233,#11234,#11235,#11236,#11237),.UNSPECIFIED.,.F.,.F.,(4,3,3,
3,3,3,3,3,3,3,3,3,3,3,3,3,3,3,3,3,3,3,3,3,3,3,3,3,3,4),(-0.378621596831286,
-0.35979753708714,-0.347859687182163,-0.339722489331693,-0.33538424950682,
-0.315512590853311,-0.301178211065556,-0.297261960366015,-0.293227388694864,
-0.272825172423111,-0.252127510483728,-0.239305021000613,-0.228805794178289,
-0.224505212292546,-0.203200653905749,-0.200837552551268,-0.18035021613173,
-0.158310724015752,-0.15433010633306,-0.150809400457636,-0.129426099231333,
-0.10759191519814,-0.0856252932872589,-0.0802029863915961,-0.0759441290511527,
-0.053396549390214,-0.0308243813684254,-0.00876573827391309,-0.00403427920390719,
0.),.UNSPECIFIED.);
#254=B_SPLINE_CURVE_WITH_KNOTS('',3,(#11238,#11239,#11240,#11241,#11242,
#11243,#11244,#11245,#11246,#11247,#11248,#11249,#11250,#11251,#11252,#11253,
#11254,#11255,#11256,#11257,#11258,#11259,#11260,#11261,#11262,#11263,#11264,
#11265,#11266,#11267,#11268,#11269,#11270,#11271,#11272,#11273,#11274,#11275,
#11276,#11277,#11278,#11279,#11280,#11281,#11282,#11283,#11284,#11285,#11286,
#11287,#11288,#11289,#11290,#11291,#11292,#11293,#11294,#11295,#11296,#11297,
#11298,#11299,#11300,#11301,#11302,#11303,#11304,#11305,#11306,#11307,#11308,
#11309,#11310,#11311,#11312,#11313,#11314,#11315,#11316,#11317,#11318,#11319,
#11320,#11321,#11322),.UNSPECIFIED.,.F.,.F.,(4,3,3,3,3,3,3,3,3,3,3,3,3,
3,3,3,3,3,3,3,3,3,3,3,3,3,3,3,4),(-0.37694081721167,-0.354634302100723,
-0.332912872548166,-0.328064580792288,-0.305815981116835,-0.290196841687263,
-0.284261051704666,-0.278600436316194,-0.256917265324022,-0.235699702105988,
-0.21494747804995,-0.20819720640224,-0.204402057236322,-0.183825922858711,
-0.180862865680265,-0.159880209104345,-0.140305785739984,-0.136021305575262,
-0.132587894912548,-0.11212857689637,-0.091763985715855,-0.0718357358806271,
-0.0676216261694051,-0.0636601282916112,-0.044102241112633,-0.0249163068456578,
-0.00635333976700777,-0.00328482218945702,0.),.UNSPECIFIED.);
#255=B_SPLINE_CURVE_WITH_KNOTS('',3,(#11324,#11325,#11326,#11327,#11328,
#11329,#11330,#11331,#11332,#11333,#11334),.UNSPECIFIED.,.F.,.F.,(4,1,1,
1,1,1,1,1,4),(15.7079632679489,15.851694142003,16.8492226764396,17.8467512108762,
18.8442797453128,19.8418082797494,20.839336814186,21.8368653486226,21.9911485751285),
 .UNSPECIFIED.);
#256=B_SPLINE_CURVE_WITH_KNOTS('',3,(#11335,#11336,#11337,#11338,#11339,
#11340,#11341,#11342,#11343,#11344),.UNSPECIFIED.,.F.,.F.,(4,1,1,1,1,1,
1,4),(15.7079632679489,16.3931980816501,17.3907266160867,18.3882551505233,
19.3857836849599,20.3833122193965,21.3808407538331,21.9911485751285),
 .UNSPECIFIED.);
#257=B_SPLINE_CURVE_WITH_KNOTS('',3,(#11761,#11762,#11763,#11764,#11765,
#11766,#11767,#11768,#11769,#11770,#11771,#11772,#11773,#11774,#11775,#11776,
#11777,#11778,#11779,#11780,#11781,#11782,#11783,#11784,#11785,#11786,#11787,
#11788,#11789,#11790,#11791,#11792,#11793,#11794,#11795,#11796,#11797,#11798,
#11799,#11800,#11801,#11802,#11803,#11804,#11805,#11806,#11807,#11808,#11809,
#11810,#11811,#11812,#11813,#11814,#11815,#11816,#11817,#11818,#11819,#11820,
#11821,#11822,#11823,#11824,#11825,#11826,#11827,#11828,#11829,#11830,#11831,
#11832,#11833,#11834,#11835,#11836,#11837,#11838,#11839,#11840,#11841,#11842),
 .UNSPECIFIED.,.F.,.F.,(4,3,3,3,3,3,3,3,3,3,3,3,3,3,3,3,3,3,3,3,3,3,3,3,
3,3,3,4),(0.,0.0185974621992716,0.0384224336108711,0.0557692835960208,0.0644714038145787,
0.0684505970799104,0.0885047587343187,0.108914678740463,0.125985317428364,
0.133848187707592,0.137284575106013,0.158359458782245,0.177197233492068,
0.197725010283636,0.205649646146363,0.209125337461315,0.230131020660481,
0.251623277314659,0.268075188611861,0.278317572045085,0.284044650132327,
0.306313638421511,0.322966021230938,0.32817264982967,0.333184030557865,
0.355705445009595,0.372923169659219,0.376940817211665),.UNSPECIFIED.);
#258=B_SPLINE_CURVE_WITH_KNOTS('',3,(#11843,#11844,#11845,#11846,#11847,
#11848,#11849,#11850,#11851,#11852,#11853,#11854,#11855,#11856,#11857,#11858,
#11859,#11860,#11861,#11862,#11863,#11864,#11865,#11866,#11867),
 .UNSPECIFIED.,.F.,.F.,(4,3,3,3,3,3,3,3,4),(-10.1295685708718,-9.97528534436599,
-8.97775680992939,-7.98022827549279,-6.98269974105619,-5.9851712066196,
-4.987642672183,-3.9901141377464,-3.84638326369226),.UNSPECIFIED.);
#259=B_SPLINE_CURVE_WITH_KNOTS('',3,(#12284,#12285,#12286,#12287,#12288,
#12289,#12290,#12291,#12292,#12293,#12294,#12295,#12296,#12297,#12298,#12299,
#12300,#12301,#12302,#12303,#12304,#12305),.UNSPECIFIED.,.F.,.F.,(4,3,3,
3,3,3,3,4),(7.59300756235152,7.9802282754928,8.9777568099294,9.97528534436599,
10.9728138788026,11.9703424132392,12.9678709476758,13.8761928695311),
 .UNSPECIFIED.);
#260=B_SPLINE_CURVE_WITH_KNOTS('',3,(#12306,#12307,#12308,#12309,#12310,
#12311,#12312,#12313,#12314,#12315,#12316,#12317,#12318,#12319,#12320,#12321,
#12322,#12323,#12324,#12325,#12326,#12327,#12328,#12329,#12330,#12331,#12332,
#12333,#12334,#12335,#12336,#12337,#12338,#12339,#12340,#12341,#12342,#12343,
#12344,#12345,#12346,#12347,#12348,#12349,#12350,#12351,#12352,#12353,#12354,
#12355,#12356,#12357,#12358,#12359,#12360,#12361,#12362,#12363,#12364,#12365,
#12366,#12367,#12368,#12369,#12370,#12371,#12372,#12373,#12374,#12375,#12376,
#12377,#12378,#12379,#12380,#12381,#12382,#12383,#12384,#12385,#12386,#12387,
#12388,#12389,#12390),.UNSPECIFIED.,.F.,.F.,(4,3,3,3,3,3,3,3,3,3,3,3,3,
3,3,3,3,3,3,3,3,3,3,3,3,3,3,3,4),(0.,0.0219660882001754,0.0445435574926492,
0.0636200527620001,0.072096934670327,0.0767543921860232,0.0810485334836077,
0.102995134794825,0.124771443916311,0.142867462849098,0.150422747843521,
0.153917793932026,0.157566639164433,0.178337409068225,0.197155519647456,
0.219426672701598,0.224328243169774,0.229401233280989,0.250066316947288,
0.270727133327362,0.285676274903019,0.296892293101634,0.3006231612417,0.320395528034006,
0.334302244254764,0.33876864872058,0.357793747762356,0.375324744080587,
0.378621596831435),.UNSPECIFIED.);
#261=B_SPLINE_CURVE_WITH_KNOTS('',3,(#12393,#12394,#12395,#12396,#12397,
#12398,#12399,#12400,#12401,#12402,#12403,#12404,#12405,#12406,#12407,#12408,
#12409,#12410,#12411,#12412,#12413,#12414,#12415,#12416,#12417,#12418,#12419,
#12420,#12421,#12422,#12423,#12424,#12425,#12426,#12427,#12428,#12429,#12430,
#12431,#12432,#12433,#12434,#12435,#12436,#12437,#12438,#12439,#12440,#12441,
#12442,#12443,#12444,#12445,#12446,#12447,#12448,#12449,#12450,#12451,#12452,
#12453,#12454,#12455,#12456,#12457,#12458,#12459,#12460,#12461,#12462,#12463,
#12464,#12465,#12466,#12467,#12468,#12469,#12470,#12471,#12472,#12473,#12474,
#12475,#12476,#12477,#12478,#12479,#12480),.UNSPECIFIED.,.F.,.F.,(4,3,3,
3,3,3,3,3,3,3,3,3,3,3,3,3,3,3,3,3,3,3,3,3,3,3,3,3,3,4),(-0.378621596831286,
-0.359797531939329,-0.347859674088644,-0.339722371887868,-0.335384191996609,
-0.315512528545638,-0.301178156546342,-0.297261836653107,-0.293227372722428,
-0.272825152816335,-0.252127491378394,-0.239305006671613,-0.228805773055512,
-0.224505205545998,-0.203200647370982,-0.200837552551268,-0.180350219633511,
-0.158310727079811,-0.154330126777592,-0.15080940414484,-0.129426105765746,
-0.107591922992953,-0.0856253011071385,-0.0802030000345852,-0.0759441337694857,
-0.0533965546995145,-0.030824386572716,-0.00876574406647046,-0.00403427920390719,
0.),.UNSPECIFIED.);
#262=B_SPLINE_CURVE_WITH_KNOTS('',3,(#12481,#12482,#12483,#12484,#12485,
#12486,#12487,#12488,#12489,#12490,#12491,#12492,#12493,#12494,#12495,#12496,
#12497,#12498,#12499,#12500,#12501,#12502,#12503,#12504,#12505,#12506,#12507,
#12508,#12509,#12510,#12511,#12512,#12513,#12514,#12515,#12516,#12517,#12518,
#12519,#12520,#12521,#12522,#12523,#12524,#12525,#12526,#12527,#12528,#12529,
#12530,#12531,#12532,#12533,#12534,#12535,#12536,#12537,#12538,#12539,#12540,
#12541,#12542,#12543,#12544,#12545,#12546,#12547,#12548,#12549,#12550,#12551,
#12552,#12553,#12554,#12555,#12556,#12557,#12558,#12559,#12560,#12561,#12562,
#12563,#12564,#12565),.UNSPECIFIED.,.F.,.F.,(4,3,3,3,3,3,3,3,3,3,3,3,3,
3,3,3,3,3,3,3,3,3,3,3,3,3,3,3,4),(-0.37694081721167,-0.354634311564495,
-0.332912880828966,-0.328064590370635,-0.305815990568489,-0.290196849957461,
-0.284261070057056,-0.278600435131014,-0.256917262572502,-0.235699695321403,
-0.214947468634417,-0.208197212481371,-0.20440205636235,-0.183825918074776,
-0.180862865680265,-0.159880209071646,-0.140305785711372,-0.136021299100323,
-0.132587889613715,-0.112128572210918,-0.091763979903476,-0.0718357249425283,
-0.0676215956084049,-0.0636601180723756,-0.0441022280989914,-0.0249162877192308,
-0.00635331060543922,-0.00328482218945702,0.),.UNSPECIFIED.);
#263=B_SPLINE_CURVE_WITH_KNOTS('',3,(#12567,#12568,#12569,#12570,#12571,
#12572,#12573,#12574,#12575,#12576,#12577),.UNSPECIFIED.,.F.,.F.,(4,1,1,
1,1,1,1,1,4),(15.7079632679489,15.851694142003,16.8492226764396,17.8467512108762,
18.8442797453128,19.8418082797494,20.839336814186,21.8368653486226,21.9911485751285),
 .UNSPECIFIED.);
#264=B_SPLINE_CURVE_WITH_KNOTS('',3,(#12578,#12579,#12580,#12581,#12582,
#12583,#12584,#12585,#12586,#12587),.UNSPECIFIED.,.F.,.F.,(4,1,1,1,1,1,
1,4),(15.7079632679489,16.3931980816501,17.3907266160867,18.3882551505233,
19.3857836849599,20.3833122193965,21.3808407538331,21.9911485751285),
 .UNSPECIFIED.);
#265=B_SPLINE_CURVE_WITH_KNOTS('',3,(#13004,#13005,#13006,#13007,#13008,
#13009,#13010,#13011,#13012,#13013,#13014,#13015,#13016,#13017,#13018,#13019,
#13020,#13021,#13022,#13023,#13024,#13025,#13026,#13027,#13028,#13029,#13030,
#13031,#13032,#13033,#13034,#13035,#13036,#13037,#13038,#13039,#13040,#13041,
#13042,#13043,#13044,#13045,#13046,#13047,#13048,#13049,#13050,#13051,#13052,
#13053,#13054,#13055,#13056,#13057,#13058,#13059,#13060,#13061,#13062,#13063,
#13064,#13065,#13066,#13067,#13068,#13069,#13070,#13071,#13072,#13073,#13074,
#13075,#13076,#13077,#13078,#13079,#13080,#13081,#13082,#13083,#13084,#13085),
 .UNSPECIFIED.,.F.,.F.,(4,3,3,3,3,3,3,3,3,3,3,3,3,3,3,3,3,3,3,3,3,3,3,3,
3,3,3,4),(0.,0.018597446670301,0.0384224200230219,0.0557692717066527,0.0644713832373243,
0.0684505917335086,0.0885047423038066,0.108914657526654,0.125985301518008,
0.133848162658074,0.137284562057273,0.158359447175397,0.177197233492068,
0.197725018062199,0.205649650255122,0.209125340384878,0.230131032726425,
0.2516232941941,0.268075184696176,0.278317563017783,0.284044652367558,0.306313641227486,
0.32296602333542,0.328172654498713,0.333184032913153,0.35570544729198,0.372923169659219,
0.376940817211665),.UNSPECIFIED.);
#266=B_SPLINE_CURVE_WITH_KNOTS('',3,(#13086,#13087,#13088,#13089,#13090,
#13091,#13092,#13093,#13094,#13095,#13096,#13097,#13098,#13099,#13100,#13101,
#13102,#13103,#13104,#13105,#13106,#13107,#13108,#13109,#13110),
 .UNSPECIFIED.,.F.,.F.,(4,3,3,3,3,3,3,3,4),(-10.1295685708718,-9.97528534436599,
-8.97775680992939,-7.98022827549279,-6.98269974105619,-5.9851712066196,
-4.987642672183,-3.9901141377464,-3.84638326369226),.UNSPECIFIED.);
#267=B_SPLINE_CURVE_WITH_KNOTS('',3,(#13527,#13528,#13529,#13530,#13531,
#13532,#13533,#13534,#13535,#13536,#13537,#13538,#13539,#13540,#13541,#13542,
#13543,#13544,#13545,#13546,#13547,#13548),.UNSPECIFIED.,.F.,.F.,(4,3,3,
3,3,3,3,4),(7.59300756235152,7.9802282754928,8.9777568099294,9.97528534436599,
10.9728138788026,11.9703424132392,12.9678709476758,13.8761928695311),
 .UNSPECIFIED.);
#268=B_SPLINE_CURVE_WITH_KNOTS('',3,(#13549,#13550,#13551,#13552,#13553,
#13554,#13555,#13556,#13557,#13558,#13559,#13560,#13561,#13562,#13563,#13564,
#13565,#13566,#13567,#13568,#13569,#13570,#13571,#13572,#13573,#13574,#13575,
#13576,#13577,#13578,#13579,#13580,#13581,#13582,#13583,#13584,#13585,#13586,
#13587,#13588,#13589,#13590,#13591,#13592,#13593,#13594,#13595,#13596,#13597,
#13598,#13599,#13600,#13601,#13602,#13603,#13604,#13605,#13606,#13607,#13608,
#13609,#13610,#13611,#13612,#13613,#13614,#13615,#13616,#13617,#13618,#13619,
#13620,#13621,#13622,#13623,#13624,#13625,#13626,#13627,#13628,#13629,#13630,
#13631,#13632,#13633),.UNSPECIFIED.,.F.,.F.,(4,3,3,3,3,3,3,3,3,3,3,3,3,
3,3,3,3,3,3,3,3,3,3,3,3,3,3,3,4),(0.,0.0219660926710697,0.0445435623967901,
0.0636200570531234,0.0720969359510079,0.0767543948971924,0.0810485342081409,
0.102995135433386,0.124771443207436,0.142867462317441,0.150422748080518,
0.153917795373617,0.157566639616675,0.178337408178314,0.197155519647456,
0.219426672701598,0.224328242817097,0.22940123326696,0.250066317110923,
0.270727133335975,0.285676270869573,0.296892286105422,0.30062315925361,
0.320395524461199,0.334302238332921,0.338768643269476,0.357793739793908,
0.375324744080587,0.378621596831435),.UNSPECIFIED.);
#269=B_SPLINE_CURVE_WITH_KNOTS('',3,(#13855,#13856,#13857,#13858),
 .UNSPECIFIED.,.F.,.F.,(4,4),(64.141416212773,64.8487979648243),
 .UNSPECIFIED.);
#270=B_SPLINE_CURVE_WITH_KNOTS('',3,(#13861,#13862,#13863,#13864,#13865,
#13866,#13867,#13868,#13869,#13870),.UNSPECIFIED.,.F.,.F.,(4,3,3,4),(-62.8318530717959,
-61.855776520294,-60.8581027054505,-60.3976421702574),.UNSPECIFIED.);
#271=B_SPLINE_CURVE_WITH_KNOTS('',3,(#13875,#13876,#13877,#13878,#13879,
#13880,#13881,#13882,#13883,#13884,#13885,#13886,#13887,#13888,#13889,#13890,
#13891,#13892,#13893,#13894,#13895,#13896,#13897,#13898,#13899),
 .UNSPECIFIED.,.F.,.F.,(4,3,3,3,3,3,3,3,4),(57.8582309055934,57.8650812609202,
58.8627550757636,59.8604288906071,60.8581027054505,61.855776520294,62.8534503351374,
63.8511241499809,64.141416212773),.UNSPECIFIED.);
#272=B_SPLINE_CURVE_WITH_KNOTS('',3,(#13900,#13901,#13902,#13903,#13904,
#13905,#13906,#13907,#13908,#13909,#13910,#13911,#13912,#13913,#13914,#13915,
#13916,#13917,#13918,#13919,#13920,#13921),.UNSPECIFIED.,.F.,.F.,(4,3,3,
3,3,3,3,4),(-60.3976421702574,-59.8604288906071,-58.8627550757636,-57.8650812609202,
-56.8674074460767,-55.8697336312333,-54.8720598163898,-54.1144568630778),
 .UNSPECIFIED.);
#273=B_SPLINE_CURVE_WITH_KNOTS('',3,(#13926,#13927,#13928,#13929,#13930,
#13931,#13932,#13933,#13934,#13935,#13936,#13937,#13938,#13939,#13940,#13941,
#13942,#13943,#13944,#13945,#13946,#13947),.UNSPECIFIED.,.F.,.F.,(4,3,3,
3,3,3,3,4),(51.5750455984138,51.8790383718595,52.8767121867029,53.8743860015464,
54.8720598163898,55.8697336312333,56.8674074460767,57.8582309055934),
 .UNSPECIFIED.);
#274=B_SPLINE_CURVE_WITH_KNOTS('',3,(#13948,#13949,#13950,#13951,#13952,
#13953,#13954,#13955,#13956,#13957,#13958,#13959,#13960,#13961,#13962,#13963,
#13964,#13965,#13966,#13967,#13968,#13969,#13970,#13971,#13972),
 .UNSPECIFIED.,.F.,.F.,(4,3,3,3,3,3,3,3,4),(-54.1144568630778,-53.8743860015464,
-52.8767121867029,-51.8790383718595,-50.881364557016,-49.8836907421725,
-48.8860169273291,-47.8883431124856,-47.8312715558982),.UNSPECIFIED.);
#275=B_SPLINE_CURVE_WITH_KNOTS('',3,(#13977,#13978,#13979,#13980,#13981,
#13982,#13983,#13984,#13985,#13986,#13987,#13988,#13989,#13990,#13991,#13992,
#13993,#13994,#13995,#13996,#13997,#13998),.UNSPECIFIED.,.F.,.F.,(4,3,3,
3,3,3,3,4),(45.2918602912342,45.8929954827987,46.8906692976422,47.8883431124856,
48.8860169273291,49.8836907421725,50.881364557016,51.5750455984138),
 .UNSPECIFIED.);
#276=B_SPLINE_CURVE_WITH_KNOTS('',3,(#13999,#14000,#14001,#14002,#14003,
#14004,#14005,#14006,#14007,#14008,#14009,#14010,#14011,#14012,#14013,#14014,
#14015,#14016,#14017,#14018,#14019,#14020),.UNSPECIFIED.,.F.,.F.,(4,3,3,
3,3,3,3,4),(-47.8312715558982,-46.8906692976422,-45.8929954827987,-44.8953216679553,
-43.8976478531118,-42.8999740382684,-41.9023002234249,-41.5480862487187),
 .UNSPECIFIED.);
#277=B_SPLINE_CURVE_WITH_KNOTS('',3,(#14025,#14026,#14027,#14028,#14029,
#14030,#14031,#14032,#14033,#14034,#14035,#14036,#14037,#14038,#14039,#14040,
#14041,#14042,#14043,#14044,#14045,#14046),.UNSPECIFIED.,.F.,.F.,(4,3,3,
3,3,3,3,4),(39.0086749840546,39.906952593738,40.9046264085815,41.9023002234249,
42.8999740382684,43.8976478531118,44.8953216679553,45.2918602912342),
 .UNSPECIFIED.);
#278=B_SPLINE_CURVE_WITH_KNOTS('',3,(#14047,#14048,#14049,#14050,#14051,
#14052,#14053,#14054,#14055,#14056,#14057,#14058,#14059,#14060,#14061,#14062,
#14063,#14064,#14065,#14066,#14067,#14068),.UNSPECIFIED.,.F.,.F.,(4,3,3,
3,3,3,3,4),(-41.5480862487187,-40.9046264085815,-39.906952593738,-38.9092787788946,
-37.9116049640511,-36.9139311492077,-35.9162573343642,-35.2649009415391),
 .UNSPECIFIED.);
#279=B_SPLINE_CURVE_WITH_KNOTS('',3,(#14073,#14074,#14075,#14076,#14077,
#14078,#14079,#14080,#14081,#14082,#14083,#14084,#14085,#14086,#14087,#14088,
#14089,#14090,#14091,#14092,#14093,#14094,#14095,#14096,#14097),
 .UNSPECIFIED.,.F.,.F.,(4,3,3,3,3,3,3,3,4),(32.725489676875,32.9232358898339,
33.9209097046773,34.9185835195208,35.9162573343642,36.9139311492077,37.9116049640511,
38.9092787788946,39.0086749840546),.UNSPECIFIED.);
#280=B_SPLINE_CURVE_WITH_KNOTS('',3,(#14098,#14099,#14100,#14101,#14102,
#14103,#14104,#14105,#14106,#14107,#14108,#14109,#14110,#14111,#14112,#14113,
#14114,#14115,#14116,#14117,#14118,#14119),.UNSPECIFIED.,.F.,.F.,(4,3,3,
3,3,3,3,4),(-35.2649009415391,-34.9185835195208,-33.9209097046773,-32.9232358898339,
-31.9255620749904,-30.927888260147,-29.9302144453035,-28.9817156343595),
 .UNSPECIFIED.);
#281=B_SPLINE_CURVE_WITH_KNOTS('',3,(#14124,#14125,#14126,#14127,#14128,
#14129,#14130,#14131,#14132,#14133,#14134,#14135,#14136,#14137,#14138,#14139,
#14140,#14141,#14142,#14143,#14144,#14145),.UNSPECIFIED.,.F.,.F.,(4,3,3,
3,3,3,3,4),(26.4423043696954,26.9371930007732,27.9348668156166,28.9325406304601,
29.9302144453035,30.927888260147,31.9255620749904,32.725489676875),
 .UNSPECIFIED.);
#282=B_SPLINE_CURVE_WITH_KNOTS('',3,(#14146,#14147,#14148,#14149,#14150,
#14151,#14152,#14153,#14154,#14155,#14156,#14157,#14158,#14159,#14160,#14161,
#14162,#14163,#14164,#14165,#14166,#14167,#14168,#14169,#14170),
 .UNSPECIFIED.,.F.,.F.,(4,3,3,3,3,3,3,3,4),(-28.9817156343595,-28.9325406304601,
-27.9348668156166,-26.9371930007732,-25.9395191859297,-24.9418453710863,
-23.9441715562428,-22.9464977413994,-22.6985303271799),.UNSPECIFIED.);
#283=B_SPLINE_CURVE_WITH_KNOTS('',3,(#14175,#14176,#14177,#14178,#14179,
#14180,#14181,#14182,#14183,#14184,#14185,#14186,#14187,#14188,#14189,#14190,
#14191,#14192,#14193,#14194,#14195,#14196),.UNSPECIFIED.,.F.,.F.,(4,3,3,
3,3,3,3,4),(20.1591190625158,20.9511501117125,21.9488239265559,22.9464977413994,
23.9441715562428,24.9418453710863,25.9395191859297,26.4423043696954),
 .UNSPECIFIED.);
#284=B_SPLINE_CURVE_WITH_KNOTS('',3,(#14197,#14198,#14199,#14200,#14201,
#14202,#14203,#14204,#14205,#14206,#14207,#14208,#14209,#14210,#14211,#14212,
#14213,#14214,#14215,#14216,#14217,#14218),.UNSPECIFIED.,.F.,.F.,(4,3,3,
3,3,3,3,4),(-22.6985303271799,-21.9488239265559,-20.9511501117125,-19.953476296869,
-18.9558024820256,-17.9581286671821,-16.9604548523387,-16.4153450200003),
 .UNSPECIFIED.);
#285=B_SPLINE_CURVE_WITH_KNOTS('',3,(#14223,#14224,#14225,#14226,#14227,
#14228,#14229,#14230,#14231,#14232,#14233,#14234,#14235,#14236,#14237,#14238,
#14239,#14240,#14241,#14242,#14243,#14244,#14245,#14246,#14247),
 .UNSPECIFIED.,.F.,.F.,(4,3,3,3,3,3,3,3,4),(13.8759337553362,13.9674334078083,
14.9651072226518,15.9627810374952,16.9604548523387,17.9581286671821,18.9558024820256,
19.953476296869,20.1591190625158),.UNSPECIFIED.);
#286=B_SPLINE_CURVE_WITH_KNOTS('',3,(#14248,#14249,#14250,#14251,#14252,
#14253,#14254,#14255,#14256,#14257,#14258,#14259,#14260,#14261,#14262,#14263,
#14264,#14265,#14266,#14267,#14268,#14269),.UNSPECIFIED.,.F.,.F.,(4,3,3,
3,3,3,3,4),(-16.4153450200003,-15.9627810374952,-14.9651072226518,-13.9674334078083,
-12.9697595929649,-11.9720857781214,-10.974411963278,-10.1321597128207),
 .UNSPECIFIED.);
#287=B_SPLINE_CURVE_WITH_KNOTS('',3,(#14275,#14276,#14277,#14278,#14279,
#14280,#14281,#14282,#14283,#14284,#14285,#14286,#14287),.UNSPECIFIED.,
 .F.,.F.,(4,3,3,3,4),(-3.84897440564113,-2.99302144453035,-1.9953476296869,
-0.997673814843452,0.),.UNSPECIFIED.);
#288=B_SPLINE_CURVE_WITH_KNOTS('',3,(#14290,#14291,#14292,#14293,#14294,
#14295,#14296,#14297,#14298,#14299,#14300,#14301,#14302,#14303,#14304,#14305,
#14306,#14307,#14308),.UNSPECIFIED.,.F.,.F.,(4,3,3,3,3,3,4),(2.01694489302847,
2.99302144453035,3.9906952593738,4.98836907421726,5.98604288906071,6.98371670390416,
7.59274844815664),.UNSPECIFIED.);
#289=B_SPLINE_CURVE_WITH_KNOTS('',3,(#14314,#14315,#14316,#14317,#14318,
#14319,#14320,#14321),.UNSPECIFIED.,.F.,.F.,(4,1,1,1,1,4),(72.2566310325652,
72.7170915677583,73.7147653826018,74.7124391974452,75.7101130122887,76.7077868271321),
 .UNSPECIFIED.);
#290=B_SPLINE_CURVE_WITH_KNOTS('',3,(#14324,#14325,#14326,#14327,#14328,
#14329,#14330,#14331,#14332),.UNSPECIFIED.,.F.,.F.,(4,1,1,1,1,1,4),(72.2566310325652,
72.263481387892,73.2611552027354,74.2588290175789,75.2565028324223,76.2541766472658,
77.2302531987677),.UNSPECIFIED.);
#291=B_SPLINE_CURVE_WITH_KNOTS('',3,(#14337,#14338,#14339,#14340,#14341,
#14342,#14343,#14344,#14345,#14346),.UNSPECIFIED.,.F.,.F.,(4,1,1,1,1,1,
1,4),(65.9734457253856,66.7310486786976,67.728722493541,68.7263963083845,
69.7240701232279,70.7217439380714,71.7194177529149,72.2566310325652),
 .UNSPECIFIED.);
#292=B_SPLINE_CURVE_WITH_KNOTS('',3,(#14347,#14348,#14349,#14350,#14351,
#14352,#14353,#14354,#14355,#14356),.UNSPECIFIED.,.F.,.F.,(4,1,1,1,1,1,
1,4),(65.9734457253856,66.2774384988313,67.2751123136747,68.2727861285182,
69.2704599433616,70.2681337582051,71.2658075730485,72.2566310325652),
 .UNSPECIFIED.);
#293=B_SPLINE_CURVE_WITH_KNOTS('',3,(#14361,#14362,#14363,#14364,#14365,
#14366,#14367,#14368,#14369,#14370,#14371),.UNSPECIFIED.,.F.,.F.,(4,1,1,
1,1,1,1,1,4),(59.6902604182061,59.7473319747934,60.7450057896369,61.7426796044803,
62.7403534193238,63.7380272341672,64.7357010490107,65.7333748638542,65.9734457253856),
 .UNSPECIFIED.);
#294=B_SPLINE_CURVE_WITH_KNOTS('',3,(#14372,#14373,#14374,#14375,#14376,
#14377,#14378,#14379,#14380,#14381),.UNSPECIFIED.,.F.,.F.,(4,1,1,1,1,1,
1,4),(59.6902604182061,60.2913956097706,61.289069424614,62.2867432394575,
63.2844170543009,64.2820908691444,65.2797646839878,65.9734457253856),
 .UNSPECIFIED.);
#295=B_SPLINE_CURVE_WITH_KNOTS('',3,(#14386,#14387,#14388,#14389,#14390,
#14391,#14392,#14393,#14394,#14395),.UNSPECIFIED.,.F.,.F.,(4,1,1,1,1,1,
1,4),(53.4070751110265,53.7612890857327,54.7589629005762,55.7566367154196,
56.7543105302631,57.7519843451065,58.74965815995,59.6902604182061),
 .UNSPECIFIED.);
#296=B_SPLINE_CURVE_WITH_KNOTS('',3,(#14396,#14397,#14398,#14399,#14400,
#14401,#14402,#14403,#14404,#14405),.UNSPECIFIED.,.F.,.F.,(4,1,1,1,1,1,
1,4),(53.4070751110265,54.3053527207099,55.3030265355533,56.3007003503968,
57.2983741652402,58.2960479800837,59.2937217949271,59.6902604182061),
 .UNSPECIFIED.);
#297=B_SPLINE_CURVE_WITH_KNOTS('',3,(#14410,#14411,#14412,#14413,#14414,
#14415,#14416,#14417,#14418,#14419),.UNSPECIFIED.,.F.,.F.,(4,1,1,1,1,1,
1,4),(47.1238898038469,47.775246196672,48.7729200115155,49.7705938263589,
50.7682676412024,51.7659414560458,52.7636152708893,53.4070751110265),
 .UNSPECIFIED.);
#298=B_SPLINE_CURVE_WITH_KNOTS('',3,(#14420,#14421,#14422,#14423,#14424,
#14425,#14426,#14427,#14428,#14429,#14430),.UNSPECIFIED.,.F.,.F.,(4,1,1,
1,1,1,1,1,4),(47.1238898038469,47.3216360168057,48.3193098316492,49.3169836464926,
50.3146574613361,51.3123312761795,52.310005091023,53.3076789058664,53.4070751110265),
 .UNSPECIFIED.);
#299=B_SPLINE_CURVE_WITH_KNOTS('',3,(#14435,#14436,#14437,#14438,#14439,
#14440,#14441,#14442,#14443,#14444),.UNSPECIFIED.,.F.,.F.,(4,1,1,1,1,1,
1,4),(40.8407044966673,41.7892033076113,42.7868771224548,43.7845509372982,
44.7822247521417,45.7798985669851,46.7775723818286,47.1238898038469),
 .UNSPECIFIED.);
#300=B_SPLINE_CURVE_WITH_KNOTS('',3,(#14445,#14446,#14447,#14448,#14449,
#14450,#14451,#14452,#14453,#14454),.UNSPECIFIED.,.F.,.F.,(4,1,1,1,1,1,
1,4),(40.8407044966673,41.335593127745,42.3332669425885,43.3309407574319,
44.3286145722754,45.3262883871188,46.3239622019623,47.1238898038469),
 .UNSPECIFIED.);
#301=B_SPLINE_CURVE_WITH_KNOTS('',3,(#14459,#14460,#14461,#14462,#14463,
#14464,#14465,#14466,#14467,#14468,#14469),.UNSPECIFIED.,.F.,.F.,(4,1,1,
1,1,1,1,1,4),(34.5575191894877,34.8054866037072,35.8031604185506,36.8008342333941,
37.7985080482375,38.796181863081,39.7938556779244,40.7915294927679,40.8407044966673),
 .UNSPECIFIED.);
#302=B_SPLINE_CURVE_WITH_KNOTS('',3,(#14470,#14471,#14472,#14473,#14474,
#14475,#14476,#14477,#14478,#14479),.UNSPECIFIED.,.F.,.F.,(4,1,1,1,1,1,
1,4),(34.5575191894877,35.3495502386843,36.3472240535278,37.3448978683712,
38.3425716832147,39.3402454980581,40.3379193129016,40.8407044966673),
 .UNSPECIFIED.);
#303=B_SPLINE_CURVE_WITH_KNOTS('',3,(#14484,#14485,#14486,#14487,#14488,
#14489,#14490,#14491,#14492,#14493),.UNSPECIFIED.,.F.,.F.,(4,1,1,1,1,1,
1,4),(28.2743338823081,28.8194437146465,29.8171175294899,30.8147913443334,
31.8124651591768,32.8101389740203,33.8078127888637,34.5575191894877),
 .UNSPECIFIED.);
#304=B_SPLINE_CURVE_WITH_KNOTS('',3,(#14494,#14495,#14496,#14497,#14498,
#14499,#14500,#14501,#14502,#14503,#14504),.UNSPECIFIED.,.F.,.F.,(4,1,1,
1,1,1,1,1,4),(28.2743338823081,28.3658335347801,29.3635073496236,30.361181164467,
31.3588549793105,32.3565287941539,33.3542026089974,34.3518764238408,34.5575191894877),
 .UNSPECIFIED.);
#305=B_SPLINE_CURVE_WITH_KNOTS('',3,(#14509,#14510,#14511,#14512,#14513,
#14514,#14515,#14516,#14517,#14518),.UNSPECIFIED.,.F.,.F.,(4,1,1,1,1,1,
1,4),(21.9911485751285,22.8334008255858,23.8310746404292,24.8287484552727,
25.8264222701161,26.8240960849596,27.821769899803,28.2743338823081),
 .UNSPECIFIED.);
#306=B_SPLINE_CURVE_WITH_KNOTS('',3,(#14519,#14520,#14521,#14522,#14523,
#14524,#14525,#14526,#14527,#14528),.UNSPECIFIED.,.F.,.F.,(4,1,1,1,1,1,
1,4),(21.9911485751285,22.3797906457194,23.3774644605629,24.3751382754063,
25.3728120902498,26.3704859050932,27.3681597199367,28.2743338823081),
 .UNSPECIFIED.);
#307=B_SPLINE_CURVE_WITH_KNOTS('',3,(#14534,#14535,#14536,#14537,#14538),
 .UNSPECIFIED.,.F.,.F.,(4,1,4),(14.3984001269718,15.3960739418153,15.7079632679489),
 .UNSPECIFIED.);
#308=B_SPLINE_CURVE_WITH_KNOTS('',3,(#14541,#14542,#14543,#14544,#14545),
 .UNSPECIFIED.,.F.,.F.,(4,1,4),(13.8759337553362,14.8520103068381,15.7079632679489),
 .UNSPECIFIED.);
#309=B_SPLINE_CURVE_WITH_KNOTS('',3,(#14571,#14572,#14573,#14574,#14575,
#14576,#14577,#14578,#14579,#14580,#14581),.UNSPECIFIED.,.F.,.F.,(4,1,1,
1,1,1,1,1,4),(15.7079632679489,15.8496841216816,16.8473579365251,17.8450317513685,
18.842705566212,19.8403793810554,20.8380531958989,21.8357270107423,21.9911485751285),
 .UNSPECIFIED.);
#310=B_SPLINE_CURVE_WITH_KNOTS('',3,(#14582,#14583,#14584,#14585,#14586,
#14587,#14588,#14589,#14590,#14591),.UNSPECIFIED.,.F.,.F.,(4,1,1,1,1,1,
1,4),(15.7079632679489,16.3937477566587,17.3914215715022,18.3890953863456,
19.3867692011891,20.3844430160325,21.382116830876,21.9911485751285),
 .UNSPECIFIED.);
#311=B_SPLINE_CURVE_WITH_KNOTS('',3,(#14864,#14865,#14866,#14867,#14868,
#14869,#14870,#14871,#14872,#14873,#14874,#14875,#14876,#14877,#14878,#14879,
#14880,#14881,#14882,#14883,#14884,#14885,#14886,#14887,#14888,#14889,#14890,
#14891,#14892,#14893,#14894,#14895,#14896,#14897,#14898,#14899,#14900,#14901,
#14902,#14903,#14904,#14905,#14906,#14907,#14908,#14909,#14910,#14911,#14912,
#14913,#14914,#14915,#14916,#14917,#14918,#14919,#14920,#14921,#14922,#14923,
#14924,#14925,#14926,#14927,#14928,#14929,#14930,#14931,#14932,#14933,#14934,
#14935,#14936,#14937,#14938,#14939,#14940,#14941,#14942,#14943,#14944,#14945,
#14946,#14947,#14948,#14949,#14950,#14951,#14952,#14953,#14954,#14955,#14956,
#14957),.UNSPECIFIED.,.F.,.F.,(4,3,3,3,3,3,3,3,3,3,3,3,3,3,3,3,3,3,3,3,
3,3,3,3,3,3,3,3,3,3,3,4),(0.,0.0297266436256191,0.060112679207304,0.0895302342422888,
0.115270594897901,0.120663503251604,0.150426428066333,0.180024192439473,
0.208881424201401,0.221328323689936,0.230189025923113,0.234057622905472,
0.262601272727233,0.290514012411483,0.295453119487182,0.324405121619328,
0.334115029800546,0.339546867385313,0.343311613769743,0.371402114253626,
0.399548690384148,0.427297276293485,0.438085418679347,0.44385539363774,
0.448937718500496,0.477641070286612,0.499168584126198,0.508042229411102,
0.513343363411791,0.539241448194656,0.563751125644958,0.56924861039943),
 .UNSPECIFIED.);
#312=B_SPLINE_CURVE_WITH_KNOTS('',3,(#14958,#14959,#14960,#14961,#14962,
#14963,#14964,#14965,#14966,#14967,#14968,#14969,#14970,#14971,#14972,#14973,
#14974,#14975,#14976,#14977,#14978,#14979,#14980,#14981,#14982,#14983,#14984,
#14985,#14986,#14987,#14988,#14989,#14990,#14991,#14992,#14993,#14994,#14995,
#14996,#14997,#14998,#14999,#15000,#15001,#15002,#15003,#15004,#15005,#15006,
#15007,#15008,#15009,#15010,#15011,#15012,#15013,#15014,#15015,#15016,#15017,
#15018,#15019,#15020,#15021,#15022,#15023,#15024,#15025,#15026,#15027,#15028,
#15029,#15030,#15031,#15032,#15033,#15034,#15035,#15036,#15037,#15038,#15039,
#15040,#15041,#15042,#15043,#15044,#15045,#15046,#15047,#15048,#15049,#15050,
#15051,#15052,#15053,#15054),.UNSPECIFIED.,.F.,.F.,(4,3,3,3,3,3,3,3,3,3,
3,3,3,3,3,3,3,3,3,3,3,3,3,3,3,3,3,3,3,3,3,3,4),(0.,0.0253663834374841,0.0514041120650232,
0.0783366031747472,0.0901195680352514,0.0965544176388419,0.102698656155734,
0.130005061278407,0.157761496023994,0.185037132253699,0.195822334387975,
0.20220621696723,0.20645540248052,0.235058614057351,0.263563013331617,0.266864040942815,
0.294770641765994,0.305810449331027,0.3111858125117,0.31568945545677,0.343780872272608,
0.372913770005713,0.40236688452419,0.41382997653101,0.422924087167126,0.42812442164653,
0.458189344870008,0.483694943608004,0.492094089615772,0.498168184514284,
0.529189962168139,0.560211739821994,0.566847306048124),.UNSPECIFIED.);
#313=B_SPLINE_CURVE_WITH_KNOTS('',3,(#15055,#15056,#15057,#15058,#15059,
#15060,#15061,#15062,#15063,#15064,#15065,#15066,#15067,#15068,#15069,#15070,
#15071,#15072,#15073,#15074,#15075,#15076,#15077,#15078,#15079),
 .UNSPECIFIED.,.F.,.F.,(4,3,3,3,3,3,3,3,4),(-10.1321597128207,-9.97673814843451,
-8.97906433359106,-7.98139051874761,-6.98371670390416,-5.9860428890607,
-4.98836907421726,-3.99069525937381,-3.84897440564113),.UNSPECIFIED.);
#314=B_SPLINE_CURVE_WITH_KNOTS('',3,(#15352,#15353,#15354,#15355,#15356,
#15357,#15358,#15359,#15360,#15361,#15362,#15363,#15364,#15365,#15366,#15367,
#15368,#15369,#15370,#15371,#15372,#15373,#15374,#15375,#15376,#15377,#15378,
#15379,#15380,#15381,#15382,#15383,#15384,#15385,#15386,#15387,#15388,#15389,
#15390,#15391,#15392,#15393,#15394,#15395,#15396,#15397,#15398,#15399,#15400,
#15401,#15402,#15403,#15404,#15405,#15406,#15407,#15408,#15409,#15410,#15411,
#15412,#15413,#15414,#15415,#15416,#15417,#15418,#15419,#15420,#15421,#15422,
#15423,#15424,#15425,#15426,#15427,#15428,#15429,#15430,#15431,#15432,#15433,
#15434,#15435,#15436,#15437,#15438,#15439,#15440,#15441,#15442,#15443,#15444,
#15445,#15446,#15447,#15448),.UNSPECIFIED.,.F.,.F.,(4,3,3,3,3,3,3,3,3,3,
3,3,3,3,3,3,3,3,3,3,3,3,3,3,3,3,3,3,3,3,3,3,4),(0.,0.0253664359602338,0.0514042119244802,
0.0783366905517712,0.0901196499512111,0.0965544540618819,0.102698644967743,
0.130005086208347,0.157761538287333,0.185037163951202,0.195822342994834,
0.20220622673851,0.206455408544716,0.235058628439391,0.26356301086795,0.266864040942809,
0.29477061610912,0.305810395174784,0.311185261381901,0.315689367741021,
0.343780744986089,0.372913624523944,0.402366734593413,0.413829681327142,
0.422920909218603,0.428124127377988,0.458189039903474,0.483694714883097,
0.492093067075374,0.498168205826972,0.529189972824469,0.560211739821966,
0.566847306048091),.UNSPECIFIED.);
#315=B_SPLINE_CURVE_WITH_KNOTS('',3,(#15449,#15450,#15451,#15452,#15453,
#15454,#15455,#15456,#15457,#15458,#15459,#15460,#15461,#15462,#15463,#15464,
#15465,#15466,#15467,#15468,#15469,#15470),.UNSPECIFIED.,.F.,.F.,(4,3,3,
3,3,3,3,4),(7.59274844815664,7.98139051874761,8.97906433359106,9.97673814843451,
10.974411963278,11.9720857781214,12.9697595929649,13.8759337553362),
 .UNSPECIFIED.);
#316=B_SPLINE_CURVE_WITH_KNOTS('',3,(#15471,#15472,#15473,#15474,#15475,
#15476,#15477,#15478,#15479,#15480,#15481,#15482,#15483,#15484,#15485,#15486,
#15487,#15488,#15489,#15490,#15491,#15492,#15493,#15494,#15495,#15496,#15497,
#15498,#15499,#15500,#15501,#15502,#15503,#15504,#15505,#15506,#15507,#15508,
#15509,#15510,#15511,#15512,#15513,#15514,#15515,#15516,#15517,#15518,#15519,
#15520,#15521,#15522,#15523,#15524,#15525,#15526,#15527,#15528,#15529,#15530,
#15531,#15532,#15533,#15534,#15535,#15536,#15537,#15538,#15539,#15540,#15541,
#15542,#15543,#15544,#15545,#15546,#15547,#15548,#15549,#15550,#15551,#15552,
#15553,#15554,#15555,#15556,#15557,#15558,#15559,#15560,#15561,#15562,#15563,
#15564),.UNSPECIFIED.,.F.,.F.,(4,3,3,3,3,3,3,3,3,3,3,3,3,3,3,3,3,3,3,3,
3,3,3,3,3,3,3,3,3,3,3,4),(0.,0.0297266875030074,0.0601127445946389,0.0895302914562022,
0.11527064496007,0.120663513700728,0.150426438565439,0.180024190458537,
0.208881422715689,0.221328316071619,0.23018892405708,0.234057477327688,
0.262601114877733,0.290513844971786,0.295453119487145,0.32440512352943,
0.334115024654919,0.339546862874593,0.343311606495589,0.371402108073593,
0.399548683927862,0.427297259020053,0.438085377485613,0.443855354480411,
0.448937716391162,0.477641068704603,0.499168582939684,0.508042210823306,
0.513343356614935,0.539241415166652,0.563751125644927,0.569248610399403),
 .UNSPECIFIED.);
#317=B_SPLINE_CURVE_WITH_KNOTS('',3,(#16050,#16051,#16052,#16053,#16054,
#16055),.UNSPECIFIED.,.F.,.F.,(4,1,1,4),(59.6902604182061,59.949285760612,
60.9492526905,61.880515305255),.UNSPECIFIED.);
#318=B_SPLINE_CURVE_WITH_KNOTS('',3,(#16058,#16059,#16060,#16061),
 .UNSPECIFIED.,.F.,.F.,(4,4),(59.6902604182061,60.6415981847469),
 .UNSPECIFIED.);
#319=B_SPLINE_CURVE_WITH_KNOTS('',3,(#16066,#16067,#16068,#16069,#16070,
#16071,#16072,#16073,#16074,#16075),.UNSPECIFIED.,.F.,.F.,(4,1,1,1,1,1,
1,4),(53.4070751110265,53.9494841812838,54.9494511111718,55.9494180410598,
56.9493849709479,57.9493519008359,58.9493188307239,59.6902604182061),
 .UNSPECIFIED.);
#320=B_SPLINE_CURVE_WITH_KNOTS('',3,(#16076,#16077,#16078,#16079,#16080,
#16081,#16082,#16083,#16084,#16085,#16086),.UNSPECIFIED.,.F.,.F.,(4,1,1,
1,1,1,1,1,4),(53.4070751110265,53.6518490548209,54.6503846448103,55.6489202347997,
56.6474558247892,57.6459914147786,58.644527004768,59.6430625947575,59.6902604182061),
 .UNSPECIFIED.);
#321=B_SPLINE_CURVE_WITH_KNOTS('',3,(#16091,#16092,#16093,#16094,#16095,
#16096,#16097,#16098,#16099,#16100),.UNSPECIFIED.,.F.,.F.,(4,1,1,1,1,1,
1,4),(47.1238898038469,47.9496826019555,48.9496495318436,49.9496164617316,
50.9495833916196,51.9495503215077,52.9495172513957,53.4070751110265),
 .UNSPECIFIED.);
#322=B_SPLINE_CURVE_WITH_KNOTS('',3,(#16101,#16102,#16103,#16104,#16105,
#16106,#16107,#16108,#16109,#16110),.UNSPECIFIED.,.F.,.F.,(4,1,1,1,1,1,
1,4),(47.1238898038469,47.6606355148843,48.6591711048737,49.6577066948632,
50.6562422848526,51.654777874842,52.6533134648314,53.4070751110265),
 .UNSPECIFIED.);
#323=B_SPLINE_CURVE_WITH_KNOTS('',3,(#16115,#16116,#16117,#16118,#16119,
#16120,#16121,#16122,#16123,#16124,#16125),.UNSPECIFIED.,.F.,.F.,(4,1,1,
1,1,1,1,1,4),(40.8407044966673,40.9499140927393,41.9498810226273,42.9498479525154,
43.9498148824034,44.9497818122914,45.9497487421795,46.9497156720675,47.1238898038469),
 .UNSPECIFIED.);
#324=B_SPLINE_CURVE_WITH_KNOTS('',3,(#16126,#16127,#16128,#16129,#16130,
#16131,#16132,#16133,#16134,#16135),.UNSPECIFIED.,.F.,.F.,(4,1,1,1,1,1,
1,4),(40.8407044966673,41.6694219749477,42.6679575649371,43.6664931549266,
44.665028744916,45.6635643349054,46.6620999248949,47.1238898038469),
 .UNSPECIFIED.);
#325=B_SPLINE_CURVE_WITH_KNOTS('',3,(#16140,#16141,#16142,#16143,#16144,
#16145,#16146,#16147,#16148,#16149),.UNSPECIFIED.,.F.,.F.,(4,1,1,1,1,1,
1,4),(34.5575191894877,34.9501125134111,35.9500794432991,36.9500463731871,
37.9500133030752,38.9499802329632,39.9499471628512,40.8407044966673),
 .UNSPECIFIED.);
#326=B_SPLINE_CURVE_WITH_KNOTS('',3,(#16150,#16151,#16152,#16153,#16154,
#16155,#16156,#16157,#16158,#16159,#16160),.UNSPECIFIED.,.F.,.F.,(4,1,1,
1,1,1,1,1,4),(34.5575191894877,34.6796728450217,35.6782084350111,36.6767440250006,
37.67527961499,38.6738152049794,39.6723507949688,40.6708863849583,40.8407044966673),
 .UNSPECIFIED.);
#327=B_SPLINE_CURVE_WITH_KNOTS('',3,(#16165,#16166,#16167,#16168,#16169,
#16170,#16171,#16172,#16173,#16174),.UNSPECIFIED.,.F.,.F.,(4,1,1,1,1,1,
1,4),(28.2743338823081,28.9503109340829,29.9502778639709,30.9502447938589,
31.950211723747,32.950178653635,33.950145583523,34.5575191894877),
 .UNSPECIFIED.);
#328=B_SPLINE_CURVE_WITH_KNOTS('',3,(#16175,#16176,#16177,#16178,#16179,
#16180,#16181,#16182,#16183,#16184),.UNSPECIFIED.,.F.,.F.,(4,1,1,1,1,1,
1,4),(28.2743338823081,28.6884593050851,29.6869948950745,30.685530485064,
31.6840660750534,32.6826016650428,33.6811372550323,34.5575191894877),
 .UNSPECIFIED.);
#329=B_SPLINE_CURVE_WITH_KNOTS('',3,(#16189,#16190,#16191,#16192,#16193,
#16194,#16195,#16196,#16197,#16198),.UNSPECIFIED.,.F.,.F.,(4,1,1,1,1,1,
1,4),(21.9911485751285,22.9505093547546,23.9504762846427,24.9504432145307,
25.9504101444187,26.9503770743068,27.9503440041948,28.2743338823081),
 .UNSPECIFIED.);
#330=B_SPLINE_CURVE_WITH_KNOTS('',3,(#16199,#16200,#16201,#16202,#16203,
#16204,#16205,#16206,#16207,#16208),.UNSPECIFIED.,.F.,.F.,(4,1,1,1,1,1,
1,4),(21.9911485751285,22.6972457651485,23.695781355138,24.6943169451274,
25.6928525351168,26.6913881251062,27.6899237150957,28.2743338823081),
 .UNSPECIFIED.);
#331=B_SPLINE_CURVE_WITH_KNOTS('',3,(#16213,#16214,#16215,#16216,#16217,
#16218,#16219,#16220,#16221,#16222,#16223),.UNSPECIFIED.,.F.,.F.,(4,1,1,
1,1,1,1,1,4),(15.707963267949,15.9507408455384,16.9507077754264,17.9506747053144,
18.9506416352025,19.9506085650905,20.9505754949786,21.9505424248666,21.9911485751285),
 .UNSPECIFIED.);
#332=B_SPLINE_CURVE_WITH_KNOTS('',3,(#16224,#16225,#16226,#16227,#16228,
#16229,#16230,#16231,#16232,#16233),.UNSPECIFIED.,.F.,.F.,(4,1,1,1,1,1,
1,4),(15.7079632679489,16.7060322252119,17.7045678152014,18.7031034051908,
19.7016389951802,20.7001745851697,21.6987101751591,21.9911485751285),
 .UNSPECIFIED.);
#333=B_SPLINE_CURVE_WITH_KNOTS('',3,(#16239,#16240,#16241,#16242,#16243,
#16244,#16245,#16246,#16247,#16248,#16249,#16250,#16251),.UNSPECIFIED.,
 .F.,.F.,(4,3,3,3,4),(-10.3761157273102,-10.3355095770483,-9.33554264716025,
-8.33557571727222,-7.9873987342723),.UNSPECIFIED.);
#334=B_SPLINE_CURVE_WITH_KNOTS('',3,(#16254,#16255,#16256,#16257,#16258,
#16259,#16260),.UNSPECIFIED.,.F.,.F.,(4,3,4),(5.91876055936317,6.401483492832,
7.40048571554784),.UNSPECIFIED.);
#335=B_SPLINE_CURVE_WITH_KNOTS('',3,(#16265,#16266,#16267,#16268,#16269,
#16270,#16271,#16272,#16273,#16274,#16275,#16276,#16277,#16278,#16279,#16280,
#16281,#16282,#16283,#16284,#16285,#16286),.UNSPECIFIED.,.F.,.F.,(4,3,3,
3,3,3,3,4),(-16.6593010344898,-16.3353111563765,-15.3353442264885,-14.3353772966004,
-13.3354103667124,-12.3354434368244,-11.3354765069363,-10.3761157273102),
 .UNSPECIFIED.);
#336=B_SPLINE_CURVE_WITH_KNOTS('',3,(#16287,#16288,#16289,#16290,#16291,
#16292,#16293,#16294,#16295,#16296,#16297,#16298,#16299,#16300,#16301,#16302,
#16303,#16304,#16305,#16306,#16307,#16308),.UNSPECIFIED.,.F.,.F.,(4,3,3,
3,3,3,3,4),(7.40048571554784,8.39855467281086,9.39709026280029,10.3956258527897,
11.3941614427792,12.3926970327686,13.391232622758,13.6836710227274),
 .UNSPECIFIED.);
#337=B_SPLINE_CURVE_WITH_KNOTS('',3,(#16313,#16314,#16315,#16316,#16317,
#16318,#16319,#16320,#16321,#16322,#16323,#16324,#16325,#16326,#16327,#16328,
#16329,#16330,#16331,#16332,#16333,#16334),.UNSPECIFIED.,.F.,.F.,(4,3,3,
3,3,3,3,4),(-22.9424863416694,-22.3351127357047,-21.3351458058167,-20.3351788759286,
-19.3352119460406,-18.3352450161526,-17.3352780862645,-16.6593010344898),
 .UNSPECIFIED.);
#338=B_SPLINE_CURVE_WITH_KNOTS('',3,(#16335,#16336,#16337,#16338,#16339,
#16340,#16341,#16342,#16343,#16344,#16345,#16346,#16347,#16348,#16349,#16350,
#16351,#16352,#16353,#16354,#16355,#16356),.UNSPECIFIED.,.F.,.F.,(4,3,3,
3,3,3,3,4),(13.6836710227274,14.3897682127475,15.3883038027369,16.3868393927263,
17.3853749827157,18.3839105727052,19.3824461626946,19.966856329907),
 .UNSPECIFIED.);
#339=B_SPLINE_CURVE_WITH_KNOTS('',3,(#16361,#16362,#16363,#16364,#16365,
#16366,#16367,#16368,#16369,#16370,#16371,#16372,#16373,#16374,#16375,#16376,
#16377,#16378,#16379,#16380,#16381,#16382),.UNSPECIFIED.,.F.,.F.,(4,3,3,
3,3,3,3,4),(-29.225671648849,-28.3349143150329,-27.3349473851449,-26.3349804552569,
-25.3350135253688,-24.3350465954808,-23.3350796655928,-22.9424863416694),
 .UNSPECIFIED.);
#340=B_SPLINE_CURVE_WITH_KNOTS('',3,(#16383,#16384,#16385,#16386,#16387,
#16388,#16389,#16390,#16391,#16392,#16393,#16394,#16395,#16396,#16397,#16398,
#16399,#16400,#16401,#16402,#16403,#16404),.UNSPECIFIED.,.F.,.F.,(4,3,3,
3,3,3,3,4),(19.966856329907,20.380981752684,21.3795173426735,22.3780529326629,
23.3765885226523,24.3751241126418,25.3736597026312,26.2500416370866),
 .UNSPECIFIED.);
#341=B_SPLINE_CURVE_WITH_KNOTS('',3,(#16409,#16410,#16411,#16412,#16413,
#16414,#16415,#16416,#16417,#16418,#16419,#16420,#16421,#16422,#16423,#16424,
#16425,#16426,#16427,#16428,#16429,#16430,#16431,#16432,#16433),
 .UNSPECIFIED.,.F.,.F.,(4,3,3,3,3,3,3,3,4),(-35.5088569560286,-35.3346828242492,
-34.3347158943612,-33.3347489644731,-32.3347820345851,-31.3348151046971,
-30.334848174809,-29.334881244921,-29.225671648849),.UNSPECIFIED.);
#342=B_SPLINE_CURVE_WITH_KNOTS('',3,(#16434,#16435,#16436,#16437,#16438,
#16439,#16440,#16441,#16442,#16443,#16444,#16445,#16446,#16447,#16448,#16449,
#16450,#16451,#16452,#16453,#16454,#16455,#16456,#16457,#16458),
 .UNSPECIFIED.,.F.,.F.,(4,3,3,3,3,3,3,3,4),(26.2500416370866,26.3721952926206,
27.37073088261,28.3692664725995,29.3678020625889,30.3663376525783,31.3648732425678,
32.3634088325572,32.5332269442662),.UNSPECIFIED.);
#343=B_SPLINE_CURVE_WITH_KNOTS('',3,(#16463,#16464,#16465,#16466,#16467,
#16468,#16469,#16470,#16471,#16472,#16473,#16474,#16475,#16476,#16477,#16478,
#16479,#16480,#16481,#16482,#16483,#16484),.UNSPECIFIED.,.F.,.F.,(4,3,3,
3,3,3,3,4),(-41.7920422632082,-41.3344844035774,-40.3345174736894,-39.3345505438013,
-38.3345836139133,-37.3346166840253,-36.3346497541372,-35.5088569560286),
 .UNSPECIFIED.);
#344=B_SPLINE_CURVE_WITH_KNOTS('',3,(#16485,#16486,#16487,#16488,#16489,
#16490,#16491,#16492,#16493,#16494,#16495,#16496,#16497,#16498,#16499,#16500,
#16501,#16502,#16503,#16504,#16505,#16506),.UNSPECIFIED.,.F.,.F.,(4,3,3,
3,3,3,3,4),(32.5332269442662,33.3619444225466,34.3604800125361,35.3590156025255,
36.3575511925149,37.3560867825044,38.3546223724938,38.8164122514458),
 .UNSPECIFIED.);
#345=B_SPLINE_CURVE_WITH_KNOTS('',3,(#16511,#16512,#16513,#16514,#16515,
#16516,#16517,#16518,#16519,#16520,#16521,#16522,#16523,#16524,#16525,#16526,
#16527,#16528,#16529,#16530,#16531,#16532),.UNSPECIFIED.,.F.,.F.,(4,3,3,
3,3,3,3,4),(-48.0752275703878,-47.3342859829056,-46.3343190530176,-45.3343521231296,
-44.3343851932415,-43.3344182633535,-42.3344513334655,-41.7920422632082),
 .UNSPECIFIED.);
#346=B_SPLINE_CURVE_WITH_KNOTS('',3,(#16533,#16534,#16535,#16536,#16537,
#16538,#16539,#16540,#16541,#16542,#16543,#16544,#16545,#16546,#16547,#16548,
#16549,#16550,#16551,#16552,#16553,#16554),.UNSPECIFIED.,.F.,.F.,(4,3,3,
3,3,3,3,4),(38.8164122514458,39.3531579624832,40.3516935524726,41.3502291424621,
42.3487647324515,43.3473003224409,44.3458359124304,45.0995975586254),
 .UNSPECIFIED.);
#347=B_SPLINE_CURVE_WITH_KNOTS('',3,(#16561,#16562,#16563,#16564,#16565,
#16566,#16567,#16568,#16569,#16570,#16571,#16572,#16573,#16574,#16575,#16576,
#16577,#16578,#16579,#16580,#16581,#16582,#16583,#16584,#16585,#16586,#16587,
#16588,#16589,#16590,#16591,#16592,#16593,#16594,#16595,#16596,#16597,#16598,
#16599,#16600,#16601,#16602,#16603,#16604,#16605,#16606,#16607,#16608,#16609,
#16610,#16611,#16612,#16613,#16614,#16615,#16616,#16617,#16618,#16619,#16620,
#16621,#16622,#16623,#16624,#16625,#16626,#16627,#16628,#16629,#16630,#16631,
#16632,#16633,#16634,#16635,#16636,#16637,#16638,#16639),.UNSPECIFIED.,
 .F.,.F.,(4,3,3,3,3,3,3,3,3,3,3,3,3,3,3,3,3,3,3,3,3,3,3,3,3,3,4),(-1.51155304937213,
-1.48679926789801,-1.46138770257497,-1.44926072615657,-1.44198354426641,
-1.43723098380472,-1.41129449679306,-1.38512818398721,-1.36854000827839,
-1.36399653483481,-1.33754097405549,-1.31123241658569,-1.28929424823319,
-1.27832516405694,-1.27239106413946,-1.267842943956,-1.26735607988068,-1.24173914861392,
-1.21547146373691,-1.18879082221463,-1.17870805215535,-1.17421497824285,
-1.17020896121405,-1.14333001988911,-1.11622858915333,-1.08943701242486,
-1.07566099703324),.UNSPECIFIED.);
#348=B_SPLINE_CURVE_WITH_KNOTS('',3,(#16642,#16643,#16644,#16645,#16646,
#16647,#16648,#16649,#16650,#16651,#16652,#16653,#16654,#16655,#16656,#16657,
#16658,#16659,#16660,#16661,#16662,#16663,#16664,#16665,#16666,#16667,#16668,
#16669,#16670,#16671,#16672,#16673,#16674,#16675,#16676,#16677,#16678,#16679,
#16680,#16681,#16682,#16683,#16684,#16685,#16686,#16687,#16688,#16689,#16690,
#16691,#16692,#16693,#16694,#16695,#16696,#16697,#16698,#16699,#16700,#16701,
#16702,#16703,#16704,#16705),.UNSPECIFIED.,.F.,.F.,(4,3,3,3,3,3,3,3,3,3,
3,3,3,3,3,3,3,3,3,3,3,4),(-0.41064875043291,-0.381298618400131,-0.351351203500698,
-0.323281054282189,-0.314112148681696,-0.307086254455368,-0.3028330734741,
-0.275277912204971,-0.261508958802399,-0.233266721972606,-0.20410838172603,
-0.199223825603653,-0.195507682996562,-0.168311322654744,-0.141222250485178,
-0.114596755830886,-0.100248696534718,-0.0960146052739596,-0.0702407882655582,
-0.0448488487084018,-0.0202028531448953,0.),.UNSPECIFIED.);
#349=B_SPLINE_CURVE_WITH_KNOTS('',3,(#16706,#16707,#16708,#16709,#16710,
#16711,#16712,#16713,#16714,#16715,#16716,#16717,#16718,#16719,#16720,#16721,
#16722,#16723,#16724,#16725,#16726,#16727,#16728,#16729,#16730,#16731,#16732,
#16733,#16734,#16735,#16736,#16737,#16738,#16739,#16740,#16741,#16742,#16743,
#16744,#16745,#16746,#16747,#16748,#16749,#16750,#16751,#16752,#16753,#16754,
#16755,#16756,#16757,#16758,#16759,#16760,#16761,#16762,#16763,#16764,#16765,
#16766,#16767,#16768,#16769,#16770,#16771,#16772,#16773,#16774,#16775,#16776,
#16777,#16778,#16779,#16780,#16781,#16782,#16783,#16784,#16785,#16786,#16787,
#16788,#16789,#16790,#16791,#16792,#16793,#16794,#16795,#16796,#16797,#16798,
#16799,#16800,#16801,#16802,#16803,#16804,#16805,#16806,#16807,#16808,#16809,
#16810,#16811,#16812,#16813,#16814,#16815,#16816,#16817,#16818,#16819,#16820,
#16821,#16822,#16823,#16824,#16825,#16826,#16827,#16828,#16829,#16830,#16831,
#16832,#16833,#16834,#16835,#16836,#16837,#16838,#16839,#16840,#16841,#16842,
#16843,#16844,#16845,#16846,#16847,#16848,#16849,#16850,#16851,#16852,#16853,
#16854,#16855,#16856,#16857,#16858,#16859,#16860,#16861,#16862,#16863,#16864,
#16865,#16866,#16867,#16868,#16869,#16870,#16871,#16872,#16873,#16874,#16875,
#16876,#16877,#16878,#16879,#16880),.UNSPECIFIED.,.F.,.F.,(4,3,3,3,3,3,
3,3,3,3,3,3,3,3,3,3,3,3,3,3,3,3,3,3,3,3,3,3,3,3,3,3,3,3,3,3,3,3,3,3,3,3,
3,3,3,3,3,3,3,3,3,3,3,3,3,3,3,3,4),(-1.07566099703324,-1.07492144342944,
-1.04755243470394,-1.02055094091712,-1.01298361676725,-0.986089044023807,
-0.977095451514633,-0.97130891557416,-0.943491786406091,-0.915956464286782,
-0.888283595509882,-0.877826699796361,-0.872194960042119,-0.86791902474336,
-0.840054061902339,-0.812175086709734,-0.784725634098613,-0.774568879849767,
-0.769117374745857,-0.765392662069162,-0.748771882229606,-0.721656701079723,
-0.693848162487506,-0.666434123134902,-0.659959284195334,-0.631746794307724,
-0.603158716171934,-0.57463751262923,-0.562124804508911,-0.556268999285474,
-0.552173232275249,-0.52328861334801,-0.494877324909424,-0.474535847666673,
-0.456784896129248,-0.448026129297894,-0.443765804674724,-0.41579810320606,
-0.386811531821062,-0.362275168226913,-0.340805850082031,-0.335237673856059,
-0.30592093381479,-0.276508451915628,-0.247512831305992,-0.23326477924646,
-0.227648927063831,-0.223354867445244,-0.193713728983455,-0.190520623067863,
-0.16154498891856,-0.132023580594298,-0.121964667371235,-0.114890334425799,
-0.110611284048844,-0.0809842299227017,-0.0509674738298579,-0.020991353997103,
0.),.UNSPECIFIED.);
#350=B_SPLINE_CURVE_WITH_KNOTS('',3,(#17094,#17095,#17096,#17097,#17098,
#17099,#17100,#17101,#17102,#17103,#17104,#17105,#17106,#17107,#17108,#17109),
 .UNSPECIFIED.,.F.,.F.,(4,3,3,3,3,4),(-52.3341206323458,-51.3341537024578,
-50.3341867725697,-49.3342198426817,-48.3342529127937,-48.0752275703878),
 .UNSPECIFIED.);
#351=B_SPLINE_CURVE_WITH_KNOTS('',3,(#17110,#17111,#17112,#17113,#17114,
#17115,#17116,#17117,#17118,#17119,#17120,#17121,#17122,#17123,#17124,#17125,
#17126,#17127,#17128,#17129,#17130,#17131,#17132,#17133,#17134,#17135,#17136,
#17137,#17138,#17139,#17140,#17141,#17142,#17143,#17144,#17145,#17146,#17147,
#17148,#17149,#17150,#17151,#17152,#17153,#17154,#17155,#17156,#17157,#17158,
#17159,#17160,#17161,#17162,#17163,#17164,#17165,#17166,#17167,#17168,#17169,
#17170,#17171,#17172,#17173,#17174,#17175,#17176,#17177,#17178,#17179,#17180,
#17181,#17182,#17183,#17184,#17185,#17186,#17187,#17188,#17189,#17190,#17191,
#17192,#17193,#17194,#17195,#17196,#17197,#17198,#17199,#17200),
 .UNSPECIFIED.,.F.,.F.,(4,3,3,3,3,3,3,3,3,3,3,3,3,3,3,3,3,3,3,3,3,3,3,3,
3,3,3,3,3,3,4),(-0.555272788399378,-0.538723215789879,-0.514041682355672,
-0.499599730599056,-0.49342192827285,-0.487658515674462,-0.461864800111998,
-0.439503006879226,-0.428741129403145,-0.42201608450083,-0.395420453364353,
-0.36730795358572,-0.340378564198256,-0.33119785145401,-0.325988107238913,
-0.32191538480378,-0.293998698163474,-0.282970454249821,-0.256042727591499,
-0.228568541876211,-0.221068540885412,-0.216710175387807,-0.188748538124756,
-0.160252201315133,-0.131521042067389,-0.114270249375622,-0.109582556703919,
-0.080105291882733,-0.0505589620440503,-0.0215888429367116,0.),
 .UNSPECIFIED.);
#352=B_SPLINE_CURVE_WITH_KNOTS('',3,(#17201,#17202,#17203,#17204,#17205),
 .UNSPECIFIED.,.F.,.F.,(4,1,4),(13.9508069857623,14.9507739156503,15.707963267949),
 .UNSPECIFIED.);
#353=B_SPLINE_CURVE_WITH_KNOTS('',3,(#17208,#17209,#17210,#17211,#17212,
#17213,#17214,#17215,#17216,#17217,#17218,#17219,#17220,#17221,#17222,#17223,
#17224,#17225,#17226),.UNSPECIFIED.,.F.,.F.,(4,3,3,3,3,3,4),(45.0995975586254,
45.3443715024198,46.3429070924092,47.3414426823987,48.3399782723881,49.3385138623775,
50.2654824574367),.UNSPECIFIED.);
#354=B_SPLINE_CURVE_WITH_KNOTS('',3,(#17469,#17470,#17471,#17472,#17473,
#17474,#17475),.UNSPECIFIED.,.F.,.F.,(4,1,1,1,4),(12.7118898652542,13.7104254552436,
14.7089610452331,15.7074966352225,15.7079632679489),.UNSPECIFIED.);
#355=B_SPLINE_CURVE_WITH_KNOTS('',3,(#17476,#17477,#17478,#17479,#17480,
#17481,#17482,#17483,#17484,#17485,#17486,#17487,#17488,#17489,#17490,#17491,
#17492,#17493,#17494,#17495,#17496,#17497,#17498,#17499,#17500,#17501,#17502,
#17503,#17504,#17505,#17506,#17507,#17508,#17509,#17510,#17511,#17512,#17513,
#17514,#17515,#17516,#17517,#17518,#17519,#17520,#17521,#17522,#17523,#17524,
#17525,#17526,#17527,#17528,#17529,#17530,#17531,#17532,#17533,#17534,#17535,
#17536,#17537,#17538,#17539,#17540,#17541,#17542,#17543,#17544,#17545,#17546,
#17547,#17548,#17549,#17550,#17551,#17552,#17553,#17554,#17555,#17556,#17557,
#17558,#17559,#17560,#17561,#17562,#17563,#17564,#17565,#17566,#17567,#17568,
#17569),.UNSPECIFIED.,.F.,.F.,(4,3,3,3,3,3,3,3,3,3,3,3,3,3,3,3,3,3,3,3,
3,3,3,3,3,3,3,3,3,3,3,4),(-0.552745378375102,-0.531732216109439,-0.502362244303788,
-0.486751274029585,-0.47919381479264,-0.472092376850761,-0.443038187382735,
-0.41923175394946,-0.408411546733614,-0.40204664346163,-0.397482113487408,
-0.369174564086956,-0.340027603044351,-0.312908274838589,-0.297482292749206,
-0.291421604682611,-0.264618441213068,-0.252586719916534,-0.225223404144207,
-0.197070478626181,-0.192533381808034,-0.188242179715238,-0.161600763841001,
-0.135001424894818,-0.108828494157218,-0.0998954833093976,-0.0942242094331416,
-0.0901853384386338,-0.0646415418758646,-0.0395000449170096,-0.0151426917384623,
0.),.UNSPECIFIED.);
#356=B_SPLINE_CURVE_WITH_KNOTS('',3,(#17593,#17594,#17595,#17596,#17597,
#17598,#17599,#17600,#17601,#17602),.UNSPECIFIED.,.F.,.F.,(4,3,3,4),(-4.09254174883832,
-3.98934747117026,-2.99201060337769,-2.06514013327813),.UNSPECIFIED.);
#357=B_SPLINE_CURVE_WITH_KNOTS('',3,(#17605,#17606,#17607,#17608,#17609,
#17610,#17611),.UNSPECIFIED.,.F.,.F.,(4,3,4),(0.,0.998146826386724,1.11419103802952),
 .UNSPECIFIED.);
#358=B_SPLINE_CURVE_WITH_KNOTS('',3,(#17616,#17617,#17618,#17619,#17620,
#17621,#17622,#17623,#17624,#17625,#17626,#17627,#17628,#17629,#17630,#17631,
#17632,#17633,#17634,#17635,#17636,#17637),.UNSPECIFIED.,.F.,.F.,(4,3,3,
3,3,3,3,4),(-10.3757270560179,-9.97336867792565,-8.97603181013308,-7.97869494234052,
-6.98135807454796,-5.98402120675539,-4.98668433896283,-4.09254174883832),
 .UNSPECIFIED.);
#359=B_SPLINE_CURVE_WITH_KNOTS('',3,(#17638,#17639,#17640,#17641,#17642,
#17643,#17644,#17645,#17646,#17647,#17648,#17649,#17650,#17651,#17652,#17653,
#17654,#17655,#17656,#17657,#17658,#17659),.UNSPECIFIED.,.F.,.F.,(4,3,3,
3,3,3,3,4),(1.11419103802952,1.99629365277347,2.9944404791602,3.99258730554694,
4.99073413193368,5.98888095832042,6.98702778470716,7.39737634520911),
 .UNSPECIFIED.);
#360=B_SPLINE_CURVE_WITH_KNOTS('',3,(#17664,#17665,#17666,#17667,#17668,
#17669,#17670,#17671,#17672,#17673,#17674,#17675,#17676,#17677,#17678,#17679,
#17680,#17681,#17682,#17683,#17684,#17685),.UNSPECIFIED.,.F.,.F.,(4,3,3,
3,3,3,3,4),(-16.6589123631975,-15.957389884681,-14.9600530168885,-13.9627161490959,
-12.9653792813033,-11.9680424135108,-10.9707055457182,-10.3757270560179),
 .UNSPECIFIED.);
#361=B_SPLINE_CURVE_WITH_KNOTS('',3,(#17686,#17687,#17688,#17689,#17690,
#17691,#17692,#17693,#17694,#17695,#17696,#17697,#17698,#17699,#17700,#17701,
#17702,#17703,#17704,#17705,#17706,#17707),.UNSPECIFIED.,.F.,.F.,(4,3,3,
3,3,3,3,4),(7.39737634520911,7.9851746110939,8.98332143748063,9.98146826386737,
10.9796150902541,11.9777619166408,12.9759087430276,13.6805616523887),
 .UNSPECIFIED.);
#362=B_SPLINE_CURVE_WITH_KNOTS('',3,(#17712,#17713,#17714,#17715,#17716,
#17717,#17718,#17719,#17720,#17721,#17722,#17723,#17724,#17725,#17726,#17727,
#17728,#17729,#17730,#17731,#17732,#17733,#17734,#17735,#17736),
 .UNSPECIFIED.,.F.,.F.,(4,3,3,3,3,3,3,3,4),(-22.9420976703771,-22.938747959229,
-21.9414110914364,-20.9440742236439,-19.9467373558513,-18.9494004880587,
-17.9520636202662,-16.9547267524736,-16.6589123631975),.UNSPECIFIED.);
#363=B_SPLINE_CURVE_WITH_KNOTS('',3,(#17737,#17738,#17739,#17740,#17741,
#17742,#17743,#17744,#17745,#17746,#17747,#17748,#17749,#17750,#17751,#17752,
#17753,#17754,#17755,#17756,#17757,#17758),.UNSPECIFIED.,.F.,.F.,(4,3,3,
3,3,3,3,4),(13.6805616523887,13.9740555694143,14.972202395801,15.9703492221878,
16.9684960485745,17.9666428749613,18.964789701348,19.9637469595683),
 .UNSPECIFIED.);
#364=B_SPLINE_CURVE_WITH_KNOTS('',3,(#17763,#17764,#17765,#17766,#17767,
#17768,#17769,#17770,#17771,#17772,#17773,#17774,#17775,#17776,#17777,#17778,
#17779,#17780,#17781,#17782,#17783,#17784),.UNSPECIFIED.,.F.,.F.,(4,3,3,
3,3,3,3,4),(-29.2252829775567,-28.9227691659844,-27.9254322981918,-26.9280954303993,
-25.9307585626067,-24.9334216948141,-23.9360848270216,-22.9420976703771),
 .UNSPECIFIED.);
#365=B_SPLINE_CURVE_WITH_KNOTS('',3,(#17785,#17786,#17787,#17788,#17789,
#17790,#17791,#17792,#17793,#17794,#17795,#17796,#17797,#17798,#17799,#17800,
#17801,#17802,#17803,#17804,#17805,#17806),.UNSPECIFIED.,.F.,.F.,(4,3,3,
3,3,3,3,4),(19.9637469595683,20.9610833541215,21.9592301805082,22.9573770068949,
23.9555238332817,24.9536706596684,25.9518174860552,26.2469322667479),
 .UNSPECIFIED.);
#366=B_SPLINE_CURVE_WITH_KNOTS('',3,(#17811,#17812,#17813,#17814,#17815,
#17816,#17817,#17818,#17819,#17820,#17821,#17822,#17823,#17824,#17825,#17826,
#17827,#17828,#17829,#17830,#17831,#17832),.UNSPECIFIED.,.F.,.F.,(4,3,3,
3,3,3,3,4),(-35.5084682847363,-34.9067903727398,-33.9094535049472,-32.9121166371546,
-31.9147797693621,-30.9174429015695,-29.9201060337769,-29.2252829775567),
 .UNSPECIFIED.);
#367=B_SPLINE_CURVE_WITH_KNOTS('',3,(#17833,#17834,#17835,#17836,#17837,
#17838,#17839,#17840,#17841,#17842,#17843,#17844,#17845,#17846,#17847,#17848,
#17849,#17850,#17851,#17852,#17853,#17854),.UNSPECIFIED.,.F.,.F.,(4,3,3,
3,3,3,3,4),(26.2469322667479,26.9499643124419,27.9481111388286,28.9462579652154,
29.9444047916021,30.9425516179888,31.9406984443756,32.5301175739274),
 .UNSPECIFIED.);
#368=B_SPLINE_CURVE_WITH_KNOTS('',3,(#17859,#17860,#17861,#17862,#17863,
#17864,#17865,#17866,#17867,#17868,#17869,#17870,#17871,#17872,#17873,#17874,
#17875,#17876,#17877,#17878,#17879,#17880),.UNSPECIFIED.,.F.,.F.,(4,3,3,
3,3,3,3,4),(-41.7916535919158,-40.8908115794952,-39.8934747117026,-38.89613784391,
-37.8988009761175,-36.9014641083249,-35.9041272405323,-35.5084682847363),
 .UNSPECIFIED.);
#369=B_SPLINE_CURVE_WITH_KNOTS('',3,(#17881,#17882,#17883,#17884,#17885,
#17886,#17887,#17888,#17889,#17890,#17891,#17892,#17893,#17894,#17895,#17896,
#17897,#17898,#17899,#17900,#17901,#17902),.UNSPECIFIED.,.F.,.F.,(4,3,3,
3,3,3,3,4),(32.5301175739274,32.9388452707623,33.9369920971491,34.9351389235358,
35.9332857499225,36.9314325763093,37.929579402696,38.813302881107),
 .UNSPECIFIED.);
#370=B_SPLINE_CURVE_WITH_KNOTS('',3,(#17907,#17908,#17909,#17910,#17911,
#17912,#17913,#17914,#17915,#17916,#17917,#17918,#17919,#17920,#17921,#17922,
#17923,#17924,#17925,#17926,#17927,#17928,#17929,#17930,#17931),
 .UNSPECIFIED.,.F.,.F.,(4,3,3,3,3,3,3,3,4),(-48.0748388990954,-47.8721696540431,
-46.8748327862506,-45.877495918458,-44.8801590506654,-43.8828221828729,
-42.8854853150803,-41.8881484472877,-41.7916535919158),.UNSPECIFIED.);
#371=B_SPLINE_CURVE_WITH_KNOTS('',3,(#17932,#17933,#17934,#17935,#17936,
#17937,#17938,#17939,#17940,#17941,#17942,#17943,#17944,#17945,#17946,#17947,
#17948,#17949,#17950,#17951,#17952,#17953,#17954,#17955,#17956),
 .UNSPECIFIED.,.F.,.F.,(4,3,3,3,3,3,3,3,4),(38.813302881107,38.9277262290827,
39.9258730554695,40.9240198818562,41.9221667082429,42.9203135346297,43.9184603610164,
44.9166071874032,45.0964881882866),.UNSPECIFIED.);
#372=B_SPLINE_CURVE_WITH_KNOTS('',3,(#17961,#17962,#17963,#17964,#17965,
#17966,#17967,#17968,#17969,#17970,#17971,#17972,#17973,#17974,#17975,#17976,
#17977,#17978,#17979,#17980,#17981,#17982),.UNSPECIFIED.,.F.,.F.,(4,3,3,
3,3,3,3,4),(-54.358024206275,-53.8561908607985,-52.8588539930059,-51.8615171252134,
-50.8641802574208,-49.8668433896283,-48.8695065218357,-48.0748388990954),
 .UNSPECIFIED.);
#373=B_SPLINE_CURVE_WITH_KNOTS('',3,(#17983,#17984,#17985,#17986,#17987,
#17988,#17989,#17990,#17991,#17992,#17993,#17994,#17995,#17996,#17997,#17998,
#17999,#18000,#18001,#18002,#18003,#18004),.UNSPECIFIED.,.F.,.F.,(4,3,3,
3,3,3,3,4),(45.0964881882866,45.9147540137899,46.9129008401766,47.9110476665634,
48.9091944929501,49.9073413193368,50.9054881457236,51.3796734954662),
 .UNSPECIFIED.);
#374=B_SPLINE_CURVE_WITH_KNOTS('',3,(#18009,#18010,#18011,#18012,#18013,
#18014,#18015,#18016,#18017,#18018,#18019,#18020,#18021,#18022,#18023,#18024,
#18025,#18026,#18027,#18028,#18029,#18030),.UNSPECIFIED.,.F.,.F.,(4,3,3,
3,3,3,3,4),(-60.6412095134546,-59.8402120675539,-58.8428751997613,-57.8455383319688,
-56.8482014641762,-55.8508645963836,-54.8535277285911,-54.358024206275),
 .UNSPECIFIED.);
#375=B_SPLINE_CURVE_WITH_KNOTS('',3,(#18031,#18032,#18033,#18034,#18035,
#18036,#18037,#18038,#18039,#18040,#18041,#18042,#18043,#18044,#18045,#18046,
#18047,#18048,#18049,#18050,#18051,#18052),.UNSPECIFIED.,.F.,.F.,(4,3,3,
3,3,3,3,4),(51.3796734954662,51.9036349721103,52.901781798497,53.8999286248838,
54.8980754512705,55.8962222776573,56.894369104044,57.6628588026458),
 .UNSPECIFIED.);
#376=B_SPLINE_CURVE_WITH_KNOTS('',3,(#18057,#18058,#18059,#18060,#18061,
#18062,#18063,#18064,#18065,#18066,#18067,#18068,#18069,#18070,#18071,#18072,
#18073,#18074,#18075,#18076,#18077,#18078,#18079,#18080,#18081),
 .UNSPECIFIED.,.F.,.F.,(4,3,3,3,3,3,3,3,4),(-66.9243948206342,-66.8215701421018,
-65.8242332743093,-64.8268964065167,-63.8295595387242,-62.8322226709316,
-61.834885803139,-60.8375489353465,-60.6412095134546),.UNSPECIFIED.);
#377=B_SPLINE_CURVE_WITH_KNOTS('',3,(#18082,#18083,#18084,#18085,#18086,
#18087,#18088,#18089,#18090,#18091,#18092,#18093,#18094,#18095,#18096,#18097,
#18098,#18099,#18100,#18101,#18102,#18103,#18104,#18105,#18106),
 .UNSPECIFIED.,.F.,.F.,(4,3,3,3,3,3,3,3,4),(57.6628588026458,57.8925159304307,
58.8906627568175,59.8888095832042,60.8869564095909,61.8851032359777,62.8832500623644,
63.8813968887512,63.9460441098254),.UNSPECIFIED.);
#378=B_SPLINE_CURVE_WITH_KNOTS('',3,(#18111,#18112,#18113,#18114,#18115,
#18116,#18117,#18118,#18119,#18120,#18121,#18122,#18123,#18124,#18125,#18126,
#18127,#18128,#18129,#18130,#18131,#18132),.UNSPECIFIED.,.F.,.F.,(4,3,3,
3,3,3,3,4),(-73.2075801278138,-72.8055913488572,-71.8082544810647,-70.8109176132721,
-69.8135807454795,-68.816243877687,-67.8189070098944,-66.9243948206342),
 .UNSPECIFIED.);
#379=B_SPLINE_CURVE_WITH_KNOTS('',3,(#18133,#18134,#18135,#18136,#18137,
#18138,#18139,#18140,#18141,#18142,#18143,#18144,#18145,#18146,#18147,#18148,
#18149,#18150,#18151,#18152,#18153,#18154),.UNSPECIFIED.,.F.,.F.,(4,3,3,
3,3,3,3,4),(63.9460441098254,64.8795437151379,65.8776905415246,66.8758373679114,
67.8739841942981,68.8721310206848,69.8702778470716,70.229229417005),
 .UNSPECIFIED.);
#380=B_SPLINE_CURVE_WITH_KNOTS('',3,(#18159,#18160,#18161,#18162,#18163,
#18164,#18165,#18166,#18167,#18168,#18169,#18170,#18171,#18172,#18173,#18174,
#18175,#18176,#18177,#18178,#18179,#18180),.UNSPECIFIED.,.F.,.F.,(4,3,3,
3,3,3,3,4),(-79.4907654349934,-78.7896125556126,-77.7922756878201,-76.7949388200275,
-75.7976019522349,-74.8002650844424,-73.8029282166498,-73.2075801278138),
 .UNSPECIFIED.);
#381=B_SPLINE_CURVE_WITH_KNOTS('',3,(#18181,#18182,#18183,#18184,#18185,
#18186,#18187,#18188,#18189,#18190,#18191,#18192,#18193,#18194,#18195,#18196,
#18197,#18198,#18199,#18200,#18201,#18202),.UNSPECIFIED.,.F.,.F.,(4,3,3,
3,3,3,3,4),(70.229229417005,70.8684246734583,71.8665714998451,72.8647183262318,
73.8628651526185,74.8610119790053,75.859158805392,76.5124147241846),
 .UNSPECIFIED.);
#382=B_SPLINE_CURVE_WITH_KNOTS('',3,(#18208,#18209,#18210,#18211,#18212,
#18213,#18214,#18215,#18216),.UNSPECIFIED.,.F.,.F.,(4,1,1,1,1,1,4),(91.106186954104,
91.4023709425158,92.3997078103083,93.3970446781009,94.3943815458935,95.391718413686,
96.3890552814786),.UNSPECIFIED.);
#383=B_SPLINE_CURVE_WITH_KNOTS('',3,(#18219,#18220,#18221,#18222,#18223,
#18224,#18225,#18226),.UNSPECIFIED.,.F.,.F.,(4,1,1,1,1,4),(91.106186954104,
91.1567735128389,92.1549203392256,93.1530671656123,94.1512139919991,95.1493608183858),
 .UNSPECIFIED.);
#384=B_SPLINE_CURVE_WITH_KNOTS('',3,(#18231,#18232,#18233,#18234,#18235,
#18236,#18237,#18238,#18239,#18240),.UNSPECIFIED.,.F.,.F.,(4,1,1,1,1,1,
1,4),(84.8230016469244,85.4183497357604,86.4156866035529,87.4130234713455,
88.4103603391381,89.4076972069306,90.4050340747232,91.106186954104),
 .UNSPECIFIED.);
#385=B_SPLINE_CURVE_WITH_KNOTS('',3,(#18241,#18242,#18243,#18244,#18245,
#18246,#18247,#18248,#18249,#18250),.UNSPECIFIED.,.F.,.F.,(4,1,1,1,1,1,
1,4),(84.8230016469244,85.1678925545184,86.1660393809052,87.1641862072919,
88.1623330336787,89.1604798600654,90.1586266864521,91.106186954104),
 .UNSPECIFIED.);
#386=B_SPLINE_CURVE_WITH_KNOTS('',3,(#18255,#18256,#18257,#18258,#18259,
#18260,#18261,#18262,#18263,#18264),.UNSPECIFIED.,.F.,.F.,(4,1,1,1,1,1,
1,4),(78.5398163397448,79.434328529005,80.4316653967976,81.4290022645901,
82.4263391323827,83.4236760001752,84.4210128679678,84.8230016469244),
 .UNSPECIFIED.);
#387=B_SPLINE_CURVE_WITH_KNOTS('',3,(#18265,#18266,#18267,#18268,#18269,
#18270,#18271,#18272,#18273,#18274),.UNSPECIFIED.,.F.,.F.,(4,1,1,1,1,1,
1,4),(78.5398163397448,79.179011596198,80.1771584225848,81.1753052489715,
82.1734520753582,83.171598901745,84.1697457281317,84.8230016469244),
 .UNSPECIFIED.);
#388=B_SPLINE_CURVE_WITH_KNOTS('',3,(#18279,#18280,#18281,#18282,#18283,
#18284,#18285,#18286,#18287,#18288,#18289),.UNSPECIFIED.,.F.,.F.,(4,1,1,
1,1,1,1,1,4),(72.2566310325652,72.452970454457,73.4503073222496,74.4476441900422,
75.4449810578347,76.4423179256273,77.4396547934198,78.4369916612124,78.5398163397448),
 .UNSPECIFIED.);
#389=B_SPLINE_CURVE_WITH_KNOTS('',3,(#18290,#18291,#18292,#18293,#18294,
#18295,#18296,#18297,#18298,#18299),.UNSPECIFIED.,.F.,.F.,(4,1,1,1,1,1,
1,4),(72.2566310325652,73.1901306378776,74.1882774642643,75.1864242906511,
76.1845711170378,77.1827179434245,78.1808647698113,78.5398163397448),
 .UNSPECIFIED.);
#390=B_SPLINE_CURVE_WITH_KNOTS('',3,(#18304,#18305,#18306,#18307,#18308,
#18309,#18310,#18311,#18312,#18313),.UNSPECIFIED.,.F.,.F.,(4,1,1,1,1,1,
1,4),(65.9734457253856,66.4689492477016,67.4662861154942,68.4636229832868,
69.4609598510793,70.4582967188719,71.4556335866645,72.2566310325652),
 .UNSPECIFIED.);
#391=B_SPLINE_CURVE_WITH_KNOTS('',3,(#18314,#18315,#18316,#18317,#18318,
#18319,#18320,#18321,#18322,#18323,#18324),.UNSPECIFIED.,.F.,.F.,(4,1,1,
1,1,1,1,1,4),(65.9734457253856,66.2031028531704,67.2012496795572,68.1993965059439,
69.1975433323307,70.1956901587174,71.1938369851041,72.1919838114909,72.2566310325652),
 .UNSPECIFIED.);
#392=B_SPLINE_CURVE_WITH_KNOTS('',3,(#18329,#18330,#18331,#18332,#18333,
#18334,#18335,#18336,#18337,#18338),.UNSPECIFIED.,.F.,.F.,(4,1,1,1,1,1,
1,4),(59.690260418206,60.4849280409463,61.4822649087388,62.4796017765314,
63.4769386443239,64.4742755121165,65.4716123799091,65.9734457253856),
 .UNSPECIFIED.);
#393=B_SPLINE_CURVE_WITH_KNOTS('',3,(#18339,#18340,#18341,#18342,#18343,
#18344,#18345,#18346,#18347,#18348),.UNSPECIFIED.,.F.,.F.,(4,1,1,1,1,1,
1,4),(59.690260418206,60.21422189485,61.2123687212368,62.2105155476235,
63.2086623740102,64.206809200397,65.2049560267837,65.9734457253856),
 .UNSPECIFIED.);
#394=B_SPLINE_CURVE_WITH_KNOTS('',3,(#18353,#18354,#18355,#18356,#18357,
#18358,#18359,#18360,#18361,#18362,#18363),.UNSPECIFIED.,.F.,.F.,(4,1,1,
1,1,1,1,1,4),(53.4070751110265,53.5035699663983,54.5009068341909,55.4982437019834,
56.495580569776,57.4929174375686,58.4902543053611,59.4875911731537,59.690260418206),
 .UNSPECIFIED.);
#395=B_SPLINE_CURVE_WITH_KNOTS('',3,(#18364,#18365,#18366,#18367,#18368,
#18369,#18370,#18371,#18372,#18373),.UNSPECIFIED.,.F.,.F.,(4,1,1,1,1,1,
1,4),(53.4070751110264,54.2253409365296,55.2234877629163,56.2216345893031,
57.2197814156898,58.2179282420766,59.2160750684633,59.690260418206),
 .UNSPECIFIED.);
#396=B_SPLINE_CURVE_WITH_KNOTS('',3,(#18378,#18379,#18380,#18381,#18382,
#18383,#18384,#18385,#18386,#18387),.UNSPECIFIED.,.F.,.F.,(4,1,1,1,1,1,
1,4),(47.1238898038469,47.5195487596429,48.5168856274355,49.514222495228,
50.5115593630206,51.5088962308132,52.5062330986057,53.4070751110265),
 .UNSPECIFIED.);
#397=B_SPLINE_CURVE_WITH_KNOTS('',3,(#18388,#18389,#18390,#18391,#18392,
#18393,#18394,#18395,#18396,#18397,#18398),.UNSPECIFIED.,.F.,.F.,(4,1,1,
1,1,1,1,1,4),(47.1238898038468,47.2383131518225,48.2364599782092,49.2346068045959,
50.2327536309827,51.2309004573694,52.2290472837561,53.2271941101429,53.4070751110264),
 .UNSPECIFIED.);
#398=B_SPLINE_CURVE_WITH_KNOTS('',3,(#18403,#18404,#18405,#18406,#18407,
#18408,#18409,#18410,#18411,#18412),.UNSPECIFIED.,.F.,.F.,(4,1,1,1,1,1,
1,4),(40.8407044966673,41.5355275528875,42.5328644206801,43.5302012884726,
44.5275381562652,45.5248750240578,46.5222118918503,47.1238898038469),
 .UNSPECIFIED.);
#399=B_SPLINE_CURVE_WITH_KNOTS('',3,(#18413,#18414,#18415,#18416,#18417,
#18418,#18419,#18420,#18421,#18422),.UNSPECIFIED.,.F.,.F.,(4,1,1,1,1,1,
1,4),(40.8407044966673,41.249432193502,42.2475790198888,43.2457258462755,
44.2438726726622,45.242019499049,46.2401663254357,47.1238898038468),
 .UNSPECIFIED.);
#400=B_SPLINE_CURVE_WITH_KNOTS('',3,(#18427,#18428,#18429,#18430,#18431,
#18432,#18433,#18434,#18435,#18436),.UNSPECIFIED.,.F.,.F.,(4,1,1,1,1,1,
1,4),(34.5575191894877,35.5515063461321,36.5488432139247,37.5461800817173,
38.5435169495098,39.5408538173024,40.538190685095,40.8407044966673),
 .UNSPECIFIED.);
#401=B_SPLINE_CURVE_WITH_KNOTS('',3,(#18437,#18438,#18439,#18440,#18441,
#18442,#18443,#18444,#18445,#18446),.UNSPECIFIED.,.F.,.F.,(4,1,1,1,1,1,
1,4),(34.5575191894876,35.2605512351816,36.2586980615683,37.2568448879551,
38.2549917143418,39.2531385407286,40.2512853671153,40.8407044966673),
 .UNSPECIFIED.);
#402=B_SPLINE_CURVE_WITH_KNOTS('',3,(#18451,#18452,#18453,#18454,#18455,
#18456,#18457,#18458,#18459,#18460,#18461),.UNSPECIFIED.,.F.,.F.,(4,1,1,
1,1,1,1,1,4),(28.2743338823081,28.5701482715842,29.5674851393767,30.5648220071693,
31.5621588749619,32.5594957427544,33.556832610547,34.5541694783396,34.5575191894877),
 .UNSPECIFIED.);
#403=B_SPLINE_CURVE_WITH_KNOTS('',3,(#18462,#18463,#18464,#18465,#18466,
#18467,#18468,#18469,#18470,#18471),.UNSPECIFIED.,.F.,.F.,(4,1,1,1,1,1,
1,4),(28.2743338823081,29.2716702768612,30.2698171032479,31.2679639296347,
32.2661107560214,33.2642575824081,34.2624044087949,34.5575191894876),
 .UNSPECIFIED.);
#404=B_SPLINE_CURVE_WITH_KNOTS('',3,(#18476,#18477,#18478,#18479,#18480,
#18481,#18482,#18483,#18484,#18485),.UNSPECIFIED.,.F.,.F.,(4,1,1,1,1,1,
1,4),(21.9911485751285,22.5861270648288,23.5834639326213,24.5808008004139,
25.5781376682065,26.575474535999,27.5728114037916,28.2743338823081),
 .UNSPECIFIED.);
#405=B_SPLINE_CURVE_WITH_KNOTS('',3,(#18486,#18487,#18488,#18489,#18490,
#18491,#18492,#18493,#18494,#18495,#18496),.UNSPECIFIED.,.F.,.F.,(4,1,1,
1,1,1,1,1,4),(21.9911485751285,22.284642492154,23.2827893185408,24.2809361449275,
25.2790829713142,26.277229797701,27.2753766240877,28.2735234504744,28.2743338823081),
 .UNSPECIFIED.);
#406=B_SPLINE_CURVE_WITH_KNOTS('',3,(#18501,#18502,#18503,#18504,#18505,
#18506,#18507,#18508,#18509,#18510),.UNSPECIFIED.,.F.,.F.,(4,1,1,1,1,1,
1,4),(15.7079632679489,16.6021058580734,17.599442725866,18.5967795936585,
19.5941164614511,20.5914533292437,21.5887901970362,21.9911485751285),
 .UNSPECIFIED.);
#407=B_SPLINE_CURVE_WITH_KNOTS('',3,(#18511,#18512,#18513,#18514,#18515,
#18516,#18517,#18518,#18519,#18520),.UNSPECIFIED.,.F.,.F.,(4,1,1,1,1,1,
1,4),(15.7079632679489,16.2957615338336,17.2939083602203,18.2920551866071,
19.2902020129938,20.2883488393806,21.2864956657673,21.9911485751285),
 .UNSPECIFIED.);
#408=B_SPLINE_CURVE_WITH_KNOTS('',3,(#18523,#18524,#18525,#18526,#18527,
#18528,#18529,#18530,#18531,#18532,#18533,#18534,#18535,#18536,#18537,#18538,
#18539,#18540,#18541,#18542,#18543,#18544,#18545,#18546,#18547,#18548,#18549,
#18550,#18551,#18552,#18553,#18554,#18555,#18556,#18557,#18558,#18559,#18560,
#18561,#18562,#18563,#18564,#18565,#18566,#18567,#18568,#18569,#18570,#18571,
#18572,#18573,#18574,#18575,#18576,#18577,#18578,#18579,#18580,#18581,#18582,
#18583,#18584,#18585,#18586,#18587,#18588,#18589,#18590,#18591,#18592,#18593,
#18594,#18595,#18596,#18597,#18598,#18599,#18600,#18601,#18602,#18603,#18604,
#18605,#18606,#18607,#18608,#18609,#18610,#18611,#18612,#18613,#18614,#18615,
#18616,#18617,#18618,#18619,#18620,#18621,#18622,#18623,#18624,#18625,#18626,
#18627,#18628,#18629,#18630,#18631,#18632,#18633,#18634,#18635,#18636,#18637,
#18638,#18639,#18640,#18641,#18642,#18643,#18644,#18645,#18646,#18647,#18648,
#18649,#18650,#18651,#18652,#18653,#18654,#18655,#18656,#18657,#18658,#18659,
#18660,#18661,#18662,#18663,#18664,#18665,#18666,#18667,#18668,#18669,#18670,
#18671,#18672,#18673,#18674,#18675,#18676,#18677,#18678,#18679,#18680,#18681,
#18682,#18683,#18684,#18685),.UNSPECIFIED.,.F.,.F.,(4,3,3,3,3,3,3,3,3,3,
3,3,3,3,3,3,3,3,3,3,3,3,3,3,3,3,3,3,3,3,3,3,3,3,3,3,3,3,3,3,3,3,3,3,3,3,
3,3,3,3,3,3,3,3,4),(-0.996917990983859,-0.978871687936248,-0.96110860637064,
-0.951564552512273,-0.947875257318018,-0.928946481496676,-0.909864161986251,
-0.904894692675967,-0.901793526230914,-0.882487196974259,-0.863299579085687,
-0.850033307248536,-0.842040929909056,-0.838709317247451,-0.836767035411385,
-0.818231407546695,-0.79887889956488,-0.782708868337739,-0.778189567206005,
-0.77429492151425,-0.754727508647775,-0.734919748031306,-0.718569473460416,
-0.712593983904593,-0.709109999006969,-0.689189825792525,-0.669518649747745,
-0.649842645634906,-0.64559751135709,-0.64260293594092,-0.622842747933918,
-0.602674899262203,-0.589266851632816,-0.58051316491066,-0.577021522026438,
-0.556531415549597,-0.536105697847013,-0.515758108037061,-0.510662639580459,
-0.506544813616949,-0.495410518227108,-0.475531470589818,-0.455379232363541,
-0.446467573071616,-0.440751338400796,-0.437135243079585,-0.416452388484242,
-0.395479231887803,-0.375187815110753,-0.368827535471261,-0.36537325419559,
-0.344179044892366,-0.32336231319227,-0.314313564779604,-0.304957861769162),
 .UNSPECIFIED.);
#409=B_SPLINE_CURVE_WITH_KNOTS('',3,(#18687,#18688,#18689,#18690,#18691,
#18692,#18693,#18694,#18695,#18696,#18697,#18698,#18699,#18700,#18701,#18702,
#18703,#18704,#18705,#18706,#18707,#18708,#18709,#18710,#18711,#18712,#18713,
#18714,#18715,#18716,#18717,#18718,#18719,#18720,#18721,#18722,#18723,#18724,
#18725,#18726,#18727,#18728,#18729,#18730,#18731,#18732,#18733,#18734,#18735,
#18736,#18737,#18738,#18739,#18740,#18741,#18742,#18743,#18744),
 .UNSPECIFIED.,.F.,.F.,(4,3,3,3,3,3,3,3,3,3,3,3,3,3,3,3,3,3,3,4),(-0.271362855059931,
-0.249815153611103,-0.228817936840513,-0.21475709335129,-0.20269615019584,
-0.199258579296682,-0.179079219908023,-0.172574562883619,-0.151002742523167,
-0.132127399707771,-0.128545224966699,-0.108660381316369,-0.088904641890274,
-0.0695673848931777,-0.0643977176859483,-0.0611873514593056,-0.0424333152675423,
-0.0240015440670001,-0.00610711498195276,0.),.UNSPECIFIED.);
#410=B_SPLINE_CURVE_WITH_KNOTS('',3,(#18747,#18748,#18749,#18750,#18751,
#18752,#18753,#18754,#18755,#18756,#18757,#18758,#18759,#18760,#18761,#18762,
#18763,#18764,#18765,#18766,#18767,#18768,#18769,#18770,#18771,#18772,#18773,
#18774,#18775,#18776,#18777,#18778,#18779,#18780,#18781,#18782,#18783,#18784,
#18785,#18786,#18787,#18788,#18789,#18790,#18791,#18792,#18793,#18794,#18795,
#18796,#18797,#18798,#18799,#18800,#18801,#18802,#18803,#18804,#18805,#18806,
#18807,#18808,#18809,#18810),.UNSPECIFIED.,.F.,.F.,(4,3,3,3,3,3,3,3,3,3,
3,3,3,3,3,3,3,3,3,3,3,4),(-0.304957861769162,-0.297138437894475,-0.27579526247451,
-0.25452115728438,-0.238505141940676,-0.229387728747905,-0.225368790891129,
-0.221917825979367,-0.200380627888395,-0.178797401191701,-0.157590348312134,
-0.15077543359462,-0.1472283770012,-0.12639303453475,-0.105100297430208,
-0.083375892217648,-0.0782531846850942,-0.0733795998480499,-0.0515968866484263,
-0.0295071888683422,-0.00749310652115608,0.),.UNSPECIFIED.);
#411=B_SPLINE_CURVE_WITH_KNOTS('',3,(#19167,#19168,#19169,#19170,#19171,
#19172,#19173,#19174),.UNSPECIFIED.,.F.,.F.,(4,1,1,1,1,4),(11.6154215191106,
12.6127583869031,13.6100952546957,14.6074321224883,15.6047689902808,15.7079632679489),
 .UNSPECIFIED.);
#412=B_SPLINE_CURVE_WITH_KNOTS('',3,(#19175,#19176,#19177,#19178,#19179,
#19180,#19181,#19182,#19183,#19184,#19185,#19186,#19187,#19188,#19189,#19190,
#19191,#19192,#19193,#19194,#19195,#19196,#19197,#19198,#19199,#19200,#19201,
#19202,#19203,#19204,#19205,#19206,#19207,#19208,#19209,#19210,#19211,#19212,
#19213,#19214,#19215,#19216,#19217,#19218,#19219,#19220,#19221,#19222,#19223,
#19224,#19225,#19226,#19227,#19228,#19229,#19230,#19231,#19232,#19233,#19234,
#19235,#19236,#19237,#19238,#19239,#19240,#19241,#19242,#19243,#19244,#19245,
#19246,#19247,#19248,#19249,#19250,#19251,#19252,#19253,#19254,#19255,#19256,
#19257,#19258,#19259),.UNSPECIFIED.,.F.,.F.,(4,3,3,3,3,3,3,3,3,3,3,3,3,
3,3,3,3,3,3,3,3,3,3,3,3,3,3,3,4),(-0.364629307890664,-0.350886157932352,
-0.329296891193796,-0.318978960138819,-0.313744359949613,-0.309365983727222,
-0.288043719998357,-0.272809977372963,-0.264007580396482,-0.260298494201204,
-0.239567406370511,-0.219347171290133,-0.206053823216401,-0.194877404256716,
-0.191399198693004,-0.171813503246808,-0.166173778995206,-0.145402056620805,
-0.126707179806039,-0.123380359543154,-0.103925995354622,-0.0845486906012833,
-0.0655680939453014,-0.062174737667072,-0.0589393440631834,-0.040349155528949,
-0.0220933089917935,-0.00442011167346308,0.),.UNSPECIFIED.);
#413=B_SPLINE_CURVE_WITH_KNOTS('',3,(#19260,#19261,#19262,#19263,#19264,
#19265,#19266,#19267,#19268,#19269,#19270,#19271,#19272,#19273,#19274,#19275),
 .UNSPECIFIED.,.F.,.F.,(4,3,3,3,3,4),(-83.2618462600588,-82.7789600267829,
-81.7816231589903,-80.7842862911978,-79.7869494234052,-79.4907654349934),
 .UNSPECIFIED.);
#414=B_SPLINE_CURVE_WITH_KNOTS('',3,(#19278,#19279,#19280,#19281,#19282,
#19283,#19284,#19285,#19286),.UNSPECIFIED.,.F.,.F.,(4,1,1,1,1,1,4),(10.3757270560178,
11.3050274018999,12.3031742282867,13.3013210546734,14.2994678810601,15.2976147074469,
15.7079632679489),.UNSPECIFIED.);
#415=B_SPLINE_CURVE_WITH_KNOTS('',3,(#19648,#19649,#19650,#19651,#19652,
#19653,#19654,#19655,#19656,#19657,#19658,#19659,#19660,#19661,#19662,#19663,
#19664,#19665,#19666),.UNSPECIFIED.,.F.,.F.,(4,3,3,3,3,3,4),(76.5124147241846,
76.8573056317787,77.8554524581655,78.8535992845522,79.8517461109389,80.8498929373257,
81.1967061267808),.UNSPECIFIED.);
#416=B_SPLINE_CURVE_WITH_KNOTS('',3,(#19667,#19668,#19669,#19670,#19671,
#19672,#19673,#19674,#19675,#19676,#19677,#19678,#19679,#19680,#19681,#19682,
#19683,#19684,#19685,#19686,#19687,#19688,#19689,#19690,#19691,#19692,#19693,
#19694,#19695,#19696,#19697,#19698,#19699,#19700,#19701,#19702,#19703,#19704,
#19705,#19706,#19707,#19708,#19709,#19710,#19711,#19712,#19713,#19714,#19715,
#19716,#19717,#19718,#19719,#19720,#19721,#19722,#19723,#19724,#19725,#19726,
#19727,#19728,#19729,#19730,#19731,#19732,#19733,#19734,#19735,#19736,#19737,
#19738,#19739,#19740,#19741,#19742,#19743,#19744,#19745,#19746,#19747,#19748),
 .UNSPECIFIED.,.F.,.F.,(4,3,3,3,3,3,3,3,3,3,3,3,3,3,3,3,3,3,3,3,3,3,3,3,
3,3,3,4),(-0.366397579005846,-0.355505695503922,-0.337536360352733,-0.327287439123245,
-0.321639660907082,-0.302830467228198,-0.288380955593988,-0.281239733716652,
-0.277590426350317,-0.258149250115452,-0.238331803396096,-0.225557446085701,
-0.218431814193006,-0.214861428615519,-0.194431505887542,-0.187234374154516,
-0.167529878294284,-0.147391270254625,-0.143955108128756,-0.123477740220191,
-0.102569087702513,-0.0815018425023604,-0.0762248591763458,-0.0720591440818486,
-0.0504140066563087,-0.0287210039487855,-0.00749333703700768,0.),
 .UNSPECIFIED.);
#417=SHAPE_REPRESENTATION_RELATIONSHIP('SRR','None',#19935,#436);
#418=SHAPE_REPRESENTATION_RELATIONSHIP('SRR','None',#19936,#437);
#419=SHAPE_REPRESENTATION_RELATIONSHIP('SRR','None',#19937,#438);
#420=SHAPE_REPRESENTATION_RELATIONSHIP('SRR','None',#19938,#439);
#421=SHAPE_REPRESENTATION_RELATIONSHIP('SRR','None',#19939,#440);
#422=SHAPE_REPRESENTATION_RELATIONSHIP('SRR','None',#19940,#441);
#423=SHAPE_REPRESENTATION_RELATIONSHIP('SRR','None',#19941,#442);
#424=SHAPE_REPRESENTATION_RELATIONSHIP('SRR','None',#19942,#443);
#425=SHAPE_REPRESENTATION_RELATIONSHIP('SRR','None',#19943,#444);
#426=SHAPE_REPRESENTATION_RELATIONSHIP('SRR','None',#19944,#445);
#427=SHAPE_REPRESENTATION_RELATIONSHIP('SRR','None',#19945,#446);
#428=SHAPE_REPRESENTATION_RELATIONSHIP('SRR','None',#19946,#447);
#429=SHAPE_REPRESENTATION_RELATIONSHIP('SRR','None',#19947,#448);
#430=SHAPE_REPRESENTATION_RELATIONSHIP('SRR','None',#19948,#449);
#431=SHAPE_REPRESENTATION_RELATIONSHIP('SRR','None',#19949,#450);
#432=SHAPE_REPRESENTATION_RELATIONSHIP('SRR','None',#19950,#451);
#433=SHAPE_REPRESENTATION_RELATIONSHIP('SRR','None',#19951,#452);
#434=SHAPE_REPRESENTATION_RELATIONSHIP('SRR','None',#19952,#453);
#435=SHAPE_REPRESENTATION_RELATIONSHIP('SRR','None',#19953,#454);
#436=ADVANCED_BREP_SHAPE_REPRESENTATION('',(#474),#19844);
#437=ADVANCED_BREP_SHAPE_REPRESENTATION('',(#475),#19845);
#438=ADVANCED_BREP_SHAPE_REPRESENTATION('',(#476),#19846);
#439=ADVANCED_BREP_SHAPE_REPRESENTATION('',(#477),#19847);
#440=ADVANCED_BREP_SHAPE_REPRESENTATION('',(#478),#19848);
#441=ADVANCED_BREP_SHAPE_REPRESENTATION('',(#479),#19849);
#442=ADVANCED_BREP_SHAPE_REPRESENTATION('',(#480),#19850);
#443=ADVANCED_BREP_SHAPE_REPRESENTATION('',(#481),#19851);
#444=ADVANCED_BREP_SHAPE_REPRESENTATION('',(#482),#19852);
#445=ADVANCED_BREP_SHAPE_REPRESENTATION('',(#483),#19853);
#446=ADVANCED_BREP_SHAPE_REPRESENTATION('',(#484),#19854);
#447=ADVANCED_BREP_SHAPE_REPRESENTATION('',(#485),#19855);
#448=ADVANCED_BREP_SHAPE_REPRESENTATION('',(#486),#19856);
#449=ADVANCED_BREP_SHAPE_REPRESENTATION('',(#487),#19857);
#450=ADVANCED_BREP_SHAPE_REPRESENTATION('',(#488),#19858);
#451=ADVANCED_BREP_SHAPE_REPRESENTATION('',(#489),#19859);
#452=ADVANCED_BREP_SHAPE_REPRESENTATION('',(#490),#19860);
#453=ADVANCED_BREP_SHAPE_REPRESENTATION('',(#491),#19861);
#454=ADVANCED_BREP_SHAPE_REPRESENTATION('',(#492),#19862);
#455=STYLED_ITEM('',(#20039),#474);
#456=STYLED_ITEM('',(#20040),#475);
#457=STYLED_ITEM('',(#20039),#476);
#458=STYLED_ITEM('',(#20041),#477);
#459=STYLED_ITEM('',(#20042),#478);
#460=STYLED_ITEM('',(#20042),#479);
#461=STYLED_ITEM('',(#20043),#480);
#462=STYLED_ITEM('',(#20044),#481);
#463=STYLED_ITEM('',(#20043),#482);
#464=STYLED_ITEM('',(#20043),#483);
#465=STYLED_ITEM('',(#20042),#484);
#466=STYLED_ITEM('',(#20044),#485);
#467=STYLED_ITEM('',(#20042),#486);
#468=STYLED_ITEM('',(#20043),#487);
#469=STYLED_ITEM('',(#20043),#488);
#470=STYLED_ITEM('',(#20044),#489);
#471=STYLED_ITEM('',(#20042),#490);
#472=STYLED_ITEM('',(#20042),#491);
#473=STYLED_ITEM('',(#20044),#492);
#474=MANIFOLD_SOLID_BREP('Body1',#6424);
#475=MANIFOLD_SOLID_BREP('Body1',#6425);
#476=MANIFOLD_SOLID_BREP('Body1',#6426);
#477=MANIFOLD_SOLID_BREP('Body1',#6427);
#478=MANIFOLD_SOLID_BREP('Body1',#6428);
#479=MANIFOLD_SOLID_BREP('Body1',#6429);
#480=MANIFOLD_SOLID_BREP('Body1',#6430);
#481=MANIFOLD_SOLID_BREP('Body1',#6431);
#482=MANIFOLD_SOLID_BREP('Body1',#6432);
#483=MANIFOLD_SOLID_BREP('Body1',#6433);
#484=MANIFOLD_SOLID_BREP('Body1',#6434);
#485=MANIFOLD_SOLID_BREP('Body1',#6435);
#486=MANIFOLD_SOLID_BREP('Body1',#6436);
#487=MANIFOLD_SOLID_BREP('Body1',#6437);
#488=MANIFOLD_SOLID_BREP('Body1',#6438);
#489=MANIFOLD_SOLID_BREP('Body1',#6439);
#490=MANIFOLD_SOLID_BREP('Body1',#6440);
#491=MANIFOLD_SOLID_BREP('Body1',#6441);
#492=MANIFOLD_SOLID_BREP('Body1',#6442);
#493=LINE('',#8742,#958);
#494=LINE('',#8745,#959);
#495=LINE('',#8755,#960);
#496=LINE('',#8758,#961);
#497=LINE('',#8764,#962);
#498=LINE('',#8770,#963);
#499=LINE('',#8776,#964);
#500=LINE('',#8782,#965);
#501=LINE('',#8787,#966);
#502=LINE('',#8789,#967);
#503=LINE('',#8791,#968);
#504=LINE('',#8792,#969);
#505=LINE('',#8795,#970);
#506=LINE('',#8797,#971);
#507=LINE('',#8798,#972);
#508=LINE('',#8801,#973);
#509=LINE('',#8803,#974);
#510=LINE('',#8804,#975);
#511=LINE('',#8806,#976);
#512=LINE('',#8807,#977);
#513=LINE('',#8811,#978);
#514=LINE('',#8813,#979);
#515=LINE('',#8815,#980);
#516=LINE('',#8816,#981);
#517=LINE('',#8819,#982);
#518=LINE('',#8821,#983);
#519=LINE('',#8822,#984);
#520=LINE('',#8825,#985);
#521=LINE('',#8827,#986);
#522=LINE('',#8828,#987);
#523=LINE('',#8830,#988);
#524=LINE('',#8831,#989);
#525=LINE('',#8835,#990);
#526=LINE('',#8837,#991);
#527=LINE('',#8839,#992);
#528=LINE('',#8840,#993);
#529=LINE('',#8844,#994);
#530=LINE('',#8846,#995);
#531=LINE('',#8848,#996);
#532=LINE('',#8849,#997);
#533=LINE('',#8851,#998);
#534=LINE('',#8852,#999);
#535=LINE('',#8855,#1000);
#536=LINE('',#8857,#1001);
#537=LINE('',#8858,#1002);
#538=LINE('',#8861,#1003);
#539=LINE('',#8863,#1004);
#540=LINE('',#8864,#1005);
#541=LINE('',#8867,#1006);
#542=LINE('',#8869,#1007);
#543=LINE('',#8870,#1008);
#544=LINE('',#8874,#1009);
#545=LINE('',#8876,#1010);
#546=LINE('',#8878,#1011);
#547=LINE('',#8879,#1012);
#548=LINE('',#8881,#1013);
#549=LINE('',#8882,#1014);
#550=LINE('',#8885,#1015);
#551=LINE('',#8887,#1016);
#552=LINE('',#8888,#1017);
#553=LINE('',#8892,#1018);
#554=LINE('',#8893,#1019);
#555=LINE('',#8894,#1020);
#556=LINE('',#8897,#1021);
#557=LINE('',#8898,#1022);
#558=LINE('',#8901,#1023);
#559=LINE('',#8902,#1024);
#560=LINE('',#8904,#1025);
#561=LINE('',#8910,#1026);
#562=LINE('',#8939,#1027);
#563=LINE('',#8966,#1028);
#564=LINE('',#9017,#1029);
#565=LINE('',#9065,#1030);
#566=LINE('',#9116,#1031);
#567=LINE('',#9167,#1032);
#568=LINE('',#9215,#1033);
#569=LINE('',#9263,#1034);
#570=LINE('',#9314,#1035);
#571=LINE('',#9362,#1036);
#572=LINE('',#9410,#1037);
#573=LINE('',#9461,#1038);
#574=LINE('',#9512,#1039);
#575=LINE('',#9560,#1040);
#576=LINE('',#9611,#1041);
#577=LINE('',#9650,#1042);
#578=LINE('',#9670,#1043);
#579=LINE('',#9694,#1044);
#580=LINE('',#9719,#1045);
#581=LINE('',#9744,#1046);
#582=LINE('',#9768,#1047);
#583=LINE('',#9793,#1048);
#584=LINE('',#9817,#1049);
#585=LINE('',#9842,#1050);
#586=LINE('',#9867,#1051);
#587=LINE('',#9891,#1052);
#588=LINE('',#9916,#1053);
#589=LINE('',#9940,#1054);
#590=LINE('',#9965,#1055);
#591=LINE('',#9990,#1056);
#592=LINE('',#10014,#1057);
#593=LINE('',#10031,#1058);
#594=LINE('',#10060,#1059);
#595=LINE('',#10087,#1060);
#596=LINE('',#10138,#1061);
#597=LINE('',#10186,#1062);
#598=LINE('',#10237,#1063);
#599=LINE('',#10288,#1064);
#600=LINE('',#10336,#1065);
#601=LINE('',#10384,#1066);
#602=LINE('',#10435,#1067);
#603=LINE('',#10483,#1068);
#604=LINE('',#10531,#1069);
#605=LINE('',#10582,#1070);
#606=LINE('',#10633,#1071);
#607=LINE('',#10681,#1072);
#608=LINE('',#10732,#1073);
#609=LINE('',#10771,#1074);
#610=LINE('',#10791,#1075);
#611=LINE('',#10815,#1076);
#612=LINE('',#10840,#1077);
#613=LINE('',#10865,#1078);
#614=LINE('',#10889,#1079);
#615=LINE('',#10914,#1080);
#616=LINE('',#10938,#1081);
#617=LINE('',#10963,#1082);
#618=LINE('',#10988,#1083);
#619=LINE('',#11012,#1084);
#620=LINE('',#11037,#1085);
#621=LINE('',#11061,#1086);
#622=LINE('',#11086,#1087);
#623=LINE('',#11111,#1088);
#624=LINE('',#11135,#1089);
#625=LINE('',#13641,#1090);
#626=LINE('',#13647,#1091);
#627=LINE('',#13653,#1092);
#628=LINE('',#13658,#1093);
#629=LINE('',#13660,#1094);
#630=LINE('',#13662,#1095);
#631=LINE('',#13663,#1096);
#632=LINE('',#13667,#1097);
#633=LINE('',#13669,#1098);
#634=LINE('',#13671,#1099);
#635=LINE('',#13672,#1100);
#636=LINE('',#13674,#1101);
#637=LINE('',#13675,#1102);
#638=LINE('',#13678,#1103);
#639=LINE('',#13680,#1104);
#640=LINE('',#13681,#1105);
#641=LINE('',#13684,#1106);
#642=LINE('',#13686,#1107);
#643=LINE('',#13687,#1108);
#644=LINE('',#13691,#1109);
#645=LINE('',#13693,#1110);
#646=LINE('',#13695,#1111);
#647=LINE('',#13696,#1112);
#648=LINE('',#13699,#1113);
#649=LINE('',#13701,#1114);
#650=LINE('',#13702,#1115);
#651=LINE('',#13705,#1116);
#652=LINE('',#13707,#1117);
#653=LINE('',#13708,#1118);
#654=LINE('',#13710,#1119);
#655=LINE('',#13713,#1120);
#656=LINE('',#13715,#1121);
#657=LINE('',#13717,#1122);
#658=LINE('',#13719,#1123);
#659=LINE('',#13721,#1124);
#660=LINE('',#13723,#1125);
#661=LINE('',#13725,#1126);
#662=LINE('',#13727,#1127);
#663=LINE('',#13728,#1128);
#664=LINE('',#13731,#1129);
#665=LINE('',#13733,#1130);
#666=LINE('',#13735,#1131);
#667=LINE('',#13736,#1132);
#668=LINE('',#13739,#1133);
#669=LINE('',#13741,#1134);
#670=LINE('',#13743,#1135);
#671=LINE('',#13744,#1136);
#672=LINE('',#13746,#1137);
#673=LINE('',#13747,#1138);
#674=LINE('',#13749,#1139);
#675=LINE('',#13751,#1140);
#676=LINE('',#13754,#1141);
#677=LINE('',#13756,#1142);
#678=LINE('',#13758,#1143);
#679=LINE('',#13760,#1144);
#680=LINE('',#13762,#1145);
#681=LINE('',#13764,#1146);
#682=LINE('',#13765,#1147);
#683=LINE('',#13769,#1148);
#684=LINE('',#13770,#1149);
#685=LINE('',#13771,#1150);
#686=LINE('',#13774,#1151);
#687=LINE('',#13775,#1152);
#688=LINE('',#13778,#1153);
#689=LINE('',#13779,#1154);
#690=LINE('',#13781,#1155);
#691=LINE('',#13785,#1156);
#692=LINE('',#13786,#1157);
#693=LINE('',#13787,#1158);
#694=LINE('',#13790,#1159);
#695=LINE('',#13791,#1160);
#696=LINE('',#13794,#1161);
#697=LINE('',#13795,#1162);
#698=LINE('',#13797,#1163);
#699=LINE('',#13801,#1164);
#700=LINE('',#13802,#1165);
#701=LINE('',#13804,#1166);
#702=LINE('',#13806,#1167);
#703=LINE('',#13808,#1168);
#704=LINE('',#13810,#1169);
#705=LINE('',#13811,#1170);
#706=LINE('',#13814,#1171);
#707=LINE('',#13815,#1172);
#708=LINE('',#13818,#1173);
#709=LINE('',#13820,#1174);
#710=LINE('',#13821,#1175);
#711=LINE('',#13824,#1176);
#712=LINE('',#13825,#1177);
#713=LINE('',#13828,#1178);
#714=LINE('',#13830,#1179);
#715=LINE('',#13831,#1180);
#716=LINE('',#13832,#1181);
#717=LINE('',#13834,#1182);
#718=LINE('',#13838,#1183);
#719=LINE('',#13839,#1184);
#720=LINE('',#13842,#1185);
#721=LINE('',#13843,#1186);
#722=LINE('',#13845,#1187);
#723=LINE('',#13846,#1188);
#724=LINE('',#13853,#1189);
#725=LINE('',#13874,#1190);
#726=LINE('',#13925,#1191);
#727=LINE('',#13976,#1192);
#728=LINE('',#14024,#1193);
#729=LINE('',#14072,#1194);
#730=LINE('',#14123,#1195);
#731=LINE('',#14174,#1196);
#732=LINE('',#14222,#1197);
#733=LINE('',#14273,#1198);
#734=LINE('',#14312,#1199);
#735=LINE('',#14336,#1200);
#736=LINE('',#14360,#1201);
#737=LINE('',#14385,#1202);
#738=LINE('',#14409,#1203);
#739=LINE('',#14434,#1204);
#740=LINE('',#14458,#1205);
#741=LINE('',#14483,#1206);
#742=LINE('',#14508,#1207);
#743=LINE('',#14532,#1208);
#744=LINE('',#14551,#1209);
#745=LINE('',#14554,#1210);
#746=LINE('',#14559,#1211);
#747=LINE('',#14565,#1212);
#748=LINE('',#15573,#1213);
#749=LINE('',#15579,#1214);
#750=LINE('',#15585,#1215);
#751=LINE('',#15589,#1216);
#752=LINE('',#15594,#1217);
#753=LINE('',#15598,#1218);
#754=LINE('',#15602,#1219);
#755=LINE('',#15604,#1220);
#756=LINE('',#15608,#1221);
#757=LINE('',#15612,#1222);
#758=LINE('',#15616,#1223);
#759=LINE('',#15617,#1224);
#760=LINE('',#15620,#1225);
#761=LINE('',#15621,#1226);
#762=LINE('',#15624,#1227);
#763=LINE('',#15625,#1228);
#764=LINE('',#15628,#1229);
#765=LINE('',#15629,#1230);
#766=LINE('',#15632,#1231);
#767=LINE('',#15636,#1232);
#768=LINE('',#15640,#1233);
#769=LINE('',#15643,#1234);
#770=LINE('',#15644,#1235);
#771=LINE('',#15646,#1236);
#772=LINE('',#15648,#1237);
#773=LINE('',#15650,#1238);
#774=LINE('',#15657,#1239);
#775=LINE('',#15659,#1240);
#776=LINE('',#15661,#1241);
#777=LINE('',#15662,#1242);
#778=LINE('',#15667,#1243);
#779=LINE('',#15671,#1244);
#780=LINE('',#15673,#1245);
#781=LINE('',#15674,#1246);
#782=LINE('',#15681,#1247);
#783=LINE('',#15683,#1248);
#784=LINE('',#15685,#1249);
#785=LINE('',#15686,#1250);
#786=LINE('',#15690,#1251);
#787=LINE('',#15692,#1252);
#788=LINE('',#15694,#1253);
#789=LINE('',#15695,#1254);
#790=LINE('',#15698,#1255);
#791=LINE('',#15700,#1256);
#792=LINE('',#15701,#1257);
#793=LINE('',#15703,#1258);
#794=LINE('',#15705,#1259);
#795=LINE('',#15706,#1260);
#796=LINE('',#15709,#1261);
#797=LINE('',#15710,#1262);
#798=LINE('',#15712,#1263);
#799=LINE('',#15713,#1264);
#800=LINE('',#15717,#1265);
#801=LINE('',#15719,#1266);
#802=LINE('',#15720,#1267);
#803=LINE('',#15723,#1268);
#804=LINE('',#15725,#1269);
#805=LINE('',#15726,#1270);
#806=LINE('',#15730,#1271);
#807=LINE('',#15731,#1272);
#808=LINE('',#15732,#1273);
#809=LINE('',#15736,#1274);
#810=LINE('',#15737,#1275);
#811=LINE('',#15738,#1276);
#812=LINE('',#15741,#1277);
#813=LINE('',#15743,#1278);
#814=LINE('',#15744,#1279);
#815=LINE('',#15748,#1280);
#816=LINE('',#15749,#1281);
#817=LINE('',#15751,#1282);
#818=LINE('',#15752,#1283);
#819=LINE('',#15755,#1284);
#820=LINE('',#15757,#1285);
#821=LINE('',#15758,#1286);
#822=LINE('',#15761,#1287);
#823=LINE('',#15762,#1288);
#824=LINE('',#15763,#1289);
#825=LINE('',#15765,#1290);
#826=LINE('',#15773,#1291);
#827=LINE('',#15784,#1292);
#828=LINE('',#15792,#1293);
#829=LINE('',#15796,#1294);
#830=LINE('',#15803,#1295);
#831=LINE('',#15814,#1296);
#832=LINE('',#15822,#1297);
#833=LINE('',#15826,#1298);
#834=LINE('',#15833,#1299);
#835=LINE('',#15839,#1300);
#836=LINE('',#15847,#1301);
#837=LINE('',#15849,#1302);
#838=LINE('',#15851,#1303);
#839=LINE('',#15852,#1304);
#840=LINE('',#15856,#1305);
#841=LINE('',#15858,#1306);
#842=LINE('',#15860,#1307);
#843=LINE('',#15861,#1308);
#844=LINE('',#15875,#1309);
#845=LINE('',#15881,#1310);
#846=LINE('',#15890,#1311);
#847=LINE('',#15896,#1312);
#848=LINE('',#15905,#1313);
#849=LINE('',#15911,#1314);
#850=LINE('',#15919,#1315);
#851=LINE('',#15921,#1316);
#852=LINE('',#15923,#1317);
#853=LINE('',#15924,#1318);
#854=LINE('',#15928,#1319);
#855=LINE('',#15930,#1320);
#856=LINE('',#15932,#1321);
#857=LINE('',#15933,#1322);
#858=LINE('',#15947,#1323);
#859=LINE('',#15958,#1324);
#860=LINE('',#15966,#1325);
#861=LINE('',#15970,#1326);
#862=LINE('',#15977,#1327);
#863=LINE('',#15983,#1328);
#864=LINE('',#15992,#1329);
#865=LINE('',#15998,#1330);
#866=LINE('',#16006,#1331);
#867=LINE('',#16008,#1332);
#868=LINE('',#16010,#1333);
#869=LINE('',#16011,#1334);
#870=LINE('',#16015,#1335);
#871=LINE('',#16017,#1336);
#872=LINE('',#16019,#1337);
#873=LINE('',#16020,#1338);
#874=LINE('',#16034,#1339);
#875=LINE('',#16040,#1340);
#876=LINE('',#16048,#1341);
#877=LINE('',#16065,#1342);
#878=LINE('',#16090,#1343);
#879=LINE('',#16114,#1344);
#880=LINE('',#16139,#1345);
#881=LINE('',#16164,#1346);
#882=LINE('',#16188,#1347);
#883=LINE('',#16212,#1348);
#884=LINE('',#16237,#1349);
#885=LINE('',#16264,#1350);
#886=LINE('',#16312,#1351);
#887=LINE('',#16360,#1352);
#888=LINE('',#16408,#1353);
#889=LINE('',#16462,#1354);
#890=LINE('',#16510,#1355);
#891=LINE('',#16559,#1356);
#892=LINE('',#17231,#1357);
#893=LINE('',#17233,#1358);
#894=LINE('',#17235,#1359);
#895=LINE('',#17236,#1360);
#896=LINE('',#17239,#1361);
#897=LINE('',#17241,#1362);
#898=LINE('',#17242,#1363);
#899=LINE('',#17245,#1364);
#900=LINE('',#17247,#1365);
#901=LINE('',#17248,#1366);
#902=LINE('',#17251,#1367);
#903=LINE('',#17253,#1368);
#904=LINE('',#17254,#1369);
#905=LINE('',#17257,#1370);
#906=LINE('',#17259,#1371);
#907=LINE('',#17260,#1372);
#908=LINE('',#17262,#1373);
#909=LINE('',#17263,#1374);
#910=LINE('',#17579,#1375);
#911=LINE('',#17585,#1376);
#912=LINE('',#17591,#1377);
#913=LINE('',#17615,#1378);
#914=LINE('',#17663,#1379);
#915=LINE('',#17711,#1380);
#916=LINE('',#17762,#1381);
#917=LINE('',#17810,#1382);
#918=LINE('',#17858,#1383);
#919=LINE('',#17906,#1384);
#920=LINE('',#17960,#1385);
#921=LINE('',#18008,#1386);
#922=LINE('',#18056,#1387);
#923=LINE('',#18110,#1388);
#924=LINE('',#18158,#1389);
#925=LINE('',#18206,#1390);
#926=LINE('',#18230,#1391);
#927=LINE('',#18254,#1392);
#928=LINE('',#18278,#1393);
#929=LINE('',#18303,#1394);
#930=LINE('',#18328,#1395);
#931=LINE('',#18352,#1396);
#932=LINE('',#18377,#1397);
#933=LINE('',#18402,#1398);
#934=LINE('',#18426,#1399);
#935=LINE('',#18450,#1400);
#936=LINE('',#18475,#1401);
#937=LINE('',#18500,#1402);
#938=LINE('',#18812,#1403);
#939=LINE('',#19753,#1404);
#940=LINE('',#19755,#1405);
#941=LINE('',#19757,#1406);
#942=LINE('',#19758,#1407);
#943=LINE('',#19761,#1408);
#944=LINE('',#19763,#1409);
#945=LINE('',#19764,#1410);
#946=LINE('',#19767,#1411);
#947=LINE('',#19769,#1412);
#948=LINE('',#19770,#1413);
#949=LINE('',#19773,#1414);
#950=LINE('',#19775,#1415);
#951=LINE('',#19776,#1416);
#952=LINE('',#19779,#1417);
#953=LINE('',#19781,#1418);
#954=LINE('',#19782,#1419);
#955=LINE('',#19784,#1420);
#956=LINE('',#19785,#1421);
#957=LINE('',#19792,#1422);
#958=VECTOR('',#7205,3.5);
#959=VECTOR('',#7208,2.5);
#960=VECTOR('',#7221,3.5);
#961=VECTOR('',#7224,2.5);
#962=VECTOR('',#7231,3.5);
#963=VECTOR('',#7238,3.5);
#964=VECTOR('',#7245,3.5);
#965=VECTOR('',#7252,3.5);
#966=VECTOR('',#7257,10.);
#967=VECTOR('',#7258,10.);
#968=VECTOR('',#7259,10.);
#969=VECTOR('',#7260,10.);
#970=VECTOR('',#7263,10.);
#971=VECTOR('',#7264,10.);
#972=VECTOR('',#7265,10.);
#973=VECTOR('',#7268,10.);
#974=VECTOR('',#7269,10.);
#975=VECTOR('',#7270,10.);
#976=VECTOR('',#7273,10.);
#977=VECTOR('',#7274,10.);
#978=VECTOR('',#7277,10.);
#979=VECTOR('',#7278,10.);
#980=VECTOR('',#7279,10.);
#981=VECTOR('',#7280,10.);
#982=VECTOR('',#7283,10.);
#983=VECTOR('',#7284,10.);
#984=VECTOR('',#7285,10.);
#985=VECTOR('',#7288,10.);
#986=VECTOR('',#7289,10.);
#987=VECTOR('',#7290,10.);
#988=VECTOR('',#7293,10.);
#989=VECTOR('',#7294,10.);
#990=VECTOR('',#7297,10.);
#991=VECTOR('',#7298,10.);
#992=VECTOR('',#7299,10.);
#993=VECTOR('',#7300,10.);
#994=VECTOR('',#7303,10.);
#995=VECTOR('',#7304,10.);
#996=VECTOR('',#7305,10.);
#997=VECTOR('',#7306,10.);
#998=VECTOR('',#7309,10.);
#999=VECTOR('',#7310,10.);
#1000=VECTOR('',#7313,10.);
#1001=VECTOR('',#7314,10.);
#1002=VECTOR('',#7315,10.);
#1003=VECTOR('',#7318,10.);
#1004=VECTOR('',#7319,10.);
#1005=VECTOR('',#7320,10.);
#1006=VECTOR('',#7323,10.);
#1007=VECTOR('',#7324,10.);
#1008=VECTOR('',#7325,10.);
#1009=VECTOR('',#7328,10.);
#1010=VECTOR('',#7329,10.);
#1011=VECTOR('',#7330,10.);
#1012=VECTOR('',#7331,10.);
#1013=VECTOR('',#7334,10.);
#1014=VECTOR('',#7335,10.);
#1015=VECTOR('',#7338,10.);
#1016=VECTOR('',#7339,10.);
#1017=VECTOR('',#7340,10.);
#1018=VECTOR('',#7343,10.);
#1019=VECTOR('',#7344,10.);
#1020=VECTOR('',#7345,10.);
#1021=VECTOR('',#7348,10.);
#1022=VECTOR('',#7349,10.);
#1023=VECTOR('',#7352,10.);
#1024=VECTOR('',#7353,10.);
#1025=VECTOR('',#7356,10.);
#1026=VECTOR('',#7363,2.);
#1027=VECTOR('',#7366,2.);
#1028=VECTOR('',#7371,2.);
#1029=VECTOR('',#7374,2.);
#1030=VECTOR('',#7377,2.);
#1031=VECTOR('',#7380,2.);
#1032=VECTOR('',#7383,2.);
#1033=VECTOR('',#7386,2.);
#1034=VECTOR('',#7389,2.);
#1035=VECTOR('',#7392,2.);
#1036=VECTOR('',#7395,2.);
#1037=VECTOR('',#7398,2.);
#1038=VECTOR('',#7401,2.);
#1039=VECTOR('',#7404,2.);
#1040=VECTOR('',#7407,2.);
#1041=VECTOR('',#7410,2.);
#1042=VECTOR('',#7415,2.05475);
#1043=VECTOR('',#7420,2.05475);
#1044=VECTOR('',#7423,2.05475);
#1045=VECTOR('',#7426,2.05475);
#1046=VECTOR('',#7429,2.05475);
#1047=VECTOR('',#7432,2.05475);
#1048=VECTOR('',#7435,2.05475);
#1049=VECTOR('',#7438,2.05475);
#1050=VECTOR('',#7441,2.05475);
#1051=VECTOR('',#7444,2.05475);
#1052=VECTOR('',#7447,2.05475);
#1053=VECTOR('',#7450,2.05475);
#1054=VECTOR('',#7453,2.05475);
#1055=VECTOR('',#7456,2.05475);
#1056=VECTOR('',#7459,2.05475);
#1057=VECTOR('',#7462,2.05475);
#1058=VECTOR('',#7467,2.);
#1059=VECTOR('',#7470,2.);
#1060=VECTOR('',#7475,2.);
#1061=VECTOR('',#7478,2.);
#1062=VECTOR('',#7481,2.);
#1063=VECTOR('',#7484,2.);
#1064=VECTOR('',#7487,2.);
#1065=VECTOR('',#7490,2.);
#1066=VECTOR('',#7493,2.);
#1067=VECTOR('',#7496,2.);
#1068=VECTOR('',#7499,2.);
#1069=VECTOR('',#7502,2.);
#1070=VECTOR('',#7505,2.);
#1071=VECTOR('',#7508,2.);
#1072=VECTOR('',#7511,2.);
#1073=VECTOR('',#7514,2.);
#1074=VECTOR('',#7519,2.05475);
#1075=VECTOR('',#7524,2.05475);
#1076=VECTOR('',#7527,2.05475);
#1077=VECTOR('',#7530,2.05475);
#1078=VECTOR('',#7533,2.05475);
#1079=VECTOR('',#7536,2.05475);
#1080=VECTOR('',#7539,2.05475);
#1081=VECTOR('',#7542,2.05475);
#1082=VECTOR('',#7545,2.05475);
#1083=VECTOR('',#7548,2.05475);
#1084=VECTOR('',#7551,2.05475);
#1085=VECTOR('',#7554,2.05475);
#1086=VECTOR('',#7557,2.05475);
#1087=VECTOR('',#7560,2.05475);
#1088=VECTOR('',#7563,2.05475);
#1089=VECTOR('',#7566,2.05475);
#1090=VECTOR('',#7589,2.);
#1091=VECTOR('',#7596,4.);
#1092=VECTOR('',#7603,4.);
#1093=VECTOR('',#7608,10.);
#1094=VECTOR('',#7609,10.);
#1095=VECTOR('',#7610,10.);
#1096=VECTOR('',#7611,10.);
#1097=VECTOR('',#7614,10.);
#1098=VECTOR('',#7615,10.);
#1099=VECTOR('',#7616,10.);
#1100=VECTOR('',#7617,10.);
#1101=VECTOR('',#7620,10.);
#1102=VECTOR('',#7621,10.);
#1103=VECTOR('',#7624,10.);
#1104=VECTOR('',#7625,10.);
#1105=VECTOR('',#7626,10.);
#1106=VECTOR('',#7629,10.);
#1107=VECTOR('',#7630,10.);
#1108=VECTOR('',#7631,10.);
#1109=VECTOR('',#7634,10.);
#1110=VECTOR('',#7635,10.);
#1111=VECTOR('',#7636,10.);
#1112=VECTOR('',#7637,10.);
#1113=VECTOR('',#7640,10.);
#1114=VECTOR('',#7641,10.);
#1115=VECTOR('',#7642,10.);
#1116=VECTOR('',#7645,10.);
#1117=VECTOR('',#7646,10.);
#1118=VECTOR('',#7647,10.);
#1119=VECTOR('',#7650,10.);
#1120=VECTOR('',#7653,10.);
#1121=VECTOR('',#7654,10.);
#1122=VECTOR('',#7655,10.);
#1123=VECTOR('',#7656,10.);
#1124=VECTOR('',#7657,10.);
#1125=VECTOR('',#7658,10.);
#1126=VECTOR('',#7659,10.);
#1127=VECTOR('',#7660,10.);
#1128=VECTOR('',#7661,10.);
#1129=VECTOR('',#7662,10.);
#1130=VECTOR('',#7663,10.);
#1131=VECTOR('',#7664,10.);
#1132=VECTOR('',#7665,10.);
#1133=VECTOR('',#7666,10.);
#1134=VECTOR('',#7667,10.);
#1135=VECTOR('',#7668,10.);
#1136=VECTOR('',#7669,10.);
#1137=VECTOR('',#7672,10.);
#1138=VECTOR('',#7673,10.);
#1139=VECTOR('',#7676,10.);
#1140=VECTOR('',#7679,10.);
#1141=VECTOR('',#7682,10.);
#1142=VECTOR('',#7683,10.);
#1143=VECTOR('',#7684,10.);
#1144=VECTOR('',#7685,10.);
#1145=VECTOR('',#7686,10.);
#1146=VECTOR('',#7687,10.);
#1147=VECTOR('',#7688,10.);
#1148=VECTOR('',#7691,10.);
#1149=VECTOR('',#7692,10.);
#1150=VECTOR('',#7693,10.);
#1151=VECTOR('',#7696,10.);
#1152=VECTOR('',#7697,10.);
#1153=VECTOR('',#7700,10.);
#1154=VECTOR('',#7701,10.);
#1155=VECTOR('',#7704,10.);
#1156=VECTOR('',#7707,10.);
#1157=VECTOR('',#7708,10.);
#1158=VECTOR('',#7709,10.);
#1159=VECTOR('',#7712,10.);
#1160=VECTOR('',#7713,10.);
#1161=VECTOR('',#7716,10.);
#1162=VECTOR('',#7717,10.);
#1163=VECTOR('',#7720,10.);
#1164=VECTOR('',#7723,10.);
#1165=VECTOR('',#7724,10.);
#1166=VECTOR('',#7725,10.);
#1167=VECTOR('',#7726,10.);
#1168=VECTOR('',#7727,10.);
#1169=VECTOR('',#7728,10.);
#1170=VECTOR('',#7729,10.);
#1171=VECTOR('',#7732,10.);
#1172=VECTOR('',#7733,10.);
#1173=VECTOR('',#7736,10.);
#1174=VECTOR('',#7737,10.);
#1175=VECTOR('',#7738,10.);
#1176=VECTOR('',#7741,10.);
#1177=VECTOR('',#7742,10.);
#1178=VECTOR('',#7745,10.);
#1179=VECTOR('',#7746,10.);
#1180=VECTOR('',#7747,10.);
#1181=VECTOR('',#7748,10.);
#1182=VECTOR('',#7751,10.);
#1183=VECTOR('',#7756,10.);
#1184=VECTOR('',#7757,10.);
#1185=VECTOR('',#7760,10.);
#1186=VECTOR('',#7761,10.);
#1187=VECTOR('',#7764,10.);
#1188=VECTOR('',#7765,10.);
#1189=VECTOR('',#7774,3.);
#1190=VECTOR('',#7779,3.);
#1191=VECTOR('',#7782,3.);
#1192=VECTOR('',#7785,3.);
#1193=VECTOR('',#7788,3.);
#1194=VECTOR('',#7791,3.);
#1195=VECTOR('',#7794,3.);
#1196=VECTOR('',#7797,3.);
#1197=VECTOR('',#7800,3.);
#1198=VECTOR('',#7803,3.);
#1199=VECTOR('',#7808,3.0735);
#1200=VECTOR('',#7813,3.0735);
#1201=VECTOR('',#7816,3.0735);
#1202=VECTOR('',#7819,3.0735);
#1203=VECTOR('',#7822,3.0735);
#1204=VECTOR('',#7825,3.0735);
#1205=VECTOR('',#7828,3.0735);
#1206=VECTOR('',#7831,3.0735);
#1207=VECTOR('',#7834,3.0735);
#1208=VECTOR('',#7837,3.0735);
#1209=VECTOR('',#7844,10.);
#1210=VECTOR('',#7847,10.);
#1211=VECTOR('',#7852,10.);
#1212=VECTOR('',#7859,10.);
#1213=VECTOR('',#7880,3.);
#1214=VECTOR('',#7887,3.);
#1215=VECTOR('',#7894,5.);
#1216=VECTOR('',#7899,6.);
#1217=VECTOR('',#7904,10.);
#1218=VECTOR('',#7907,10.);
#1219=VECTOR('',#7912,10.);
#1220=VECTOR('',#7913,10.);
#1221=VECTOR('',#7916,10.);
#1222=VECTOR('',#7919,10.);
#1223=VECTOR('',#7922,10.);
#1224=VECTOR('',#7923,10.);
#1225=VECTOR('',#7926,10.);
#1226=VECTOR('',#7927,10.);
#1227=VECTOR('',#7930,10.);
#1228=VECTOR('',#7931,10.);
#1229=VECTOR('',#7934,10.);
#1230=VECTOR('',#7935,10.);
#1231=VECTOR('',#7938,10.);
#1232=VECTOR('',#7941,10.);
#1233=VECTOR('',#7944,10.);
#1234=VECTOR('',#7949,10.);
#1235=VECTOR('',#7950,10.);
#1236=VECTOR('',#7953,10.);
#1237=VECTOR('',#7956,10.);
#1238=VECTOR('',#7959,10.);
#1239=VECTOR('',#7968,10.);
#1240=VECTOR('',#7969,10.);
#1241=VECTOR('',#7970,10.);
#1242=VECTOR('',#7971,10.);
#1243=VECTOR('',#7976,10.);
#1244=VECTOR('',#7981,10.);
#1245=VECTOR('',#7982,10.);
#1246=VECTOR('',#7983,10.);
#1247=VECTOR('',#7992,10.);
#1248=VECTOR('',#7993,10.);
#1249=VECTOR('',#7994,10.);
#1250=VECTOR('',#7995,10.);
#1251=VECTOR('',#7998,10.);
#1252=VECTOR('',#7999,10.);
#1253=VECTOR('',#8000,10.);
#1254=VECTOR('',#8001,10.);
#1255=VECTOR('',#8004,10.);
#1256=VECTOR('',#8005,10.);
#1257=VECTOR('',#8006,10.);
#1258=VECTOR('',#8009,10.);
#1259=VECTOR('',#8010,10.);
#1260=VECTOR('',#8011,10.);
#1261=VECTOR('',#8014,10.);
#1262=VECTOR('',#8015,10.);
#1263=VECTOR('',#8018,10.);
#1264=VECTOR('',#8019,10.);
#1265=VECTOR('',#8024,10.);
#1266=VECTOR('',#8025,10.);
#1267=VECTOR('',#8026,10.);
#1268=VECTOR('',#8029,10.);
#1269=VECTOR('',#8030,10.);
#1270=VECTOR('',#8031,10.);
#1271=VECTOR('',#8034,10.);
#1272=VECTOR('',#8035,10.);
#1273=VECTOR('',#8036,10.);
#1274=VECTOR('',#8039,10.);
#1275=VECTOR('',#8040,10.);
#1276=VECTOR('',#8041,10.);
#1277=VECTOR('',#8044,10.);
#1278=VECTOR('',#8045,10.);
#1279=VECTOR('',#8046,10.);
#1280=VECTOR('',#8049,10.);
#1281=VECTOR('',#8050,10.);
#1282=VECTOR('',#8051,10.);
#1283=VECTOR('',#8052,10.);
#1284=VECTOR('',#8055,10.);
#1285=VECTOR('',#8056,10.);
#1286=VECTOR('',#8057,10.);
#1287=VECTOR('',#8060,10.);
#1288=VECTOR('',#8061,10.);
#1289=VECTOR('',#8062,10.);
#1290=VECTOR('',#8065,10.);
#1291=VECTOR('',#8076,2.);
#1292=VECTOR('',#8091,3.);
#1293=VECTOR('',#8100,5.);
#1294=VECTOR('',#8107,3.);
#1295=VECTOR('',#8116,3.);
#1296=VECTOR('',#8131,4.);
#1297=VECTOR('',#8140,7.);
#1298=VECTOR('',#8147,4.);
#1299=VECTOR('',#8156,3.);
#1300=VECTOR('',#8163,5.);
#1301=VECTOR('',#8174,10.);
#1302=VECTOR('',#8175,10.);
#1303=VECTOR('',#8176,10.);
#1304=VECTOR('',#8177,10.);
#1305=VECTOR('',#8180,10.);
#1306=VECTOR('',#8181,10.);
#1307=VECTOR('',#8182,10.);
#1308=VECTOR('',#8183,10.);
#1309=VECTOR('',#8206,4.);
#1310=VECTOR('',#8213,5.);
#1311=VECTOR('',#8226,4.);
#1312=VECTOR('',#8233,7.);
#1313=VECTOR('',#8246,4.);
#1314=VECTOR('',#8253,8.);
#1315=VECTOR('',#8264,10.);
#1316=VECTOR('',#8265,10.);
#1317=VECTOR('',#8266,10.);
#1318=VECTOR('',#8267,10.);
#1319=VECTOR('',#8270,10.);
#1320=VECTOR('',#8271,10.);
#1321=VECTOR('',#8272,10.);
#1322=VECTOR('',#8273,10.);
#1323=VECTOR('',#8296,1.5);
#1324=VECTOR('',#8311,2.);
#1325=VECTOR('',#8320,4.);
#1326=VECTOR('',#8327,2.);
#1327=VECTOR('',#8336,2.);
#1328=VECTOR('',#8343,4.);
#1329=VECTOR('',#8356,2.);
#1330=VECTOR('',#8363,4.);
#1331=VECTOR('',#8374,10.);
#1332=VECTOR('',#8375,10.);
#1333=VECTOR('',#8376,10.);
#1334=VECTOR('',#8377,10.);
#1335=VECTOR('',#8380,10.);
#1336=VECTOR('',#8381,10.);
#1337=VECTOR('',#8382,10.);
#1338=VECTOR('',#8383,10.);
#1339=VECTOR('',#8406,4.);
#1340=VECTOR('',#8413,12.);
#1341=VECTOR('',#8424,2.37175);
#1342=VECTOR('',#8429,2.37175);
#1343=VECTOR('',#8432,2.37175);
#1344=VECTOR('',#8435,2.37175);
#1345=VECTOR('',#8438,2.37175);
#1346=VECTOR('',#8441,2.37175);
#1347=VECTOR('',#8444,2.37175);
#1348=VECTOR('',#8447,2.37175);
#1349=VECTOR('',#8450,3.);
#1350=VECTOR('',#8455,3.);
#1351=VECTOR('',#8458,3.);
#1352=VECTOR('',#8461,3.);
#1353=VECTOR('',#8464,3.);
#1354=VECTOR('',#8467,3.);
#1355=VECTOR('',#8470,3.);
#1356=VECTOR('',#8475,2.5);
#1357=VECTOR('',#8484,10.);
#1358=VECTOR('',#8485,10.);
#1359=VECTOR('',#8486,10.);
#1360=VECTOR('',#8487,10.);
#1361=VECTOR('',#8490,10.);
#1362=VECTOR('',#8491,10.);
#1363=VECTOR('',#8492,10.);
#1364=VECTOR('',#8495,10.);
#1365=VECTOR('',#8496,10.);
#1366=VECTOR('',#8497,10.);
#1367=VECTOR('',#8500,10.);
#1368=VECTOR('',#8501,10.);
#1369=VECTOR('',#8502,10.);
#1370=VECTOR('',#8505,10.);
#1371=VECTOR('',#8506,10.);
#1372=VECTOR('',#8507,10.);
#1373=VECTOR('',#8510,10.);
#1374=VECTOR('',#8511,10.);
#1375=VECTOR('',#8526,6.);
#1376=VECTOR('',#8535,4.);
#1377=VECTOR('',#8542,2.);
#1378=VECTOR('',#8547,2.);
#1379=VECTOR('',#8550,2.);
#1380=VECTOR('',#8553,2.);
#1381=VECTOR('',#8556,2.);
#1382=VECTOR('',#8559,2.);
#1383=VECTOR('',#8562,2.);
#1384=VECTOR('',#8565,2.);
#1385=VECTOR('',#8568,2.);
#1386=VECTOR('',#8571,2.);
#1387=VECTOR('',#8574,2.);
#1388=VECTOR('',#8577,2.);
#1389=VECTOR('',#8580,2.);
#1390=VECTOR('',#8583,1.5555);
#1391=VECTOR('',#8588,1.5555);
#1392=VECTOR('',#8591,1.5555);
#1393=VECTOR('',#8594,1.5555);
#1394=VECTOR('',#8597,1.5555);
#1395=VECTOR('',#8600,1.5555);
#1396=VECTOR('',#8603,1.5555);
#1397=VECTOR('',#8606,1.5555);
#1398=VECTOR('',#8609,1.5555);
#1399=VECTOR('',#8612,1.5555);
#1400=VECTOR('',#8615,1.5555);
#1401=VECTOR('',#8618,1.5555);
#1402=VECTOR('',#8621,1.5555);
#1403=VECTOR('',#8626,1.5);
#1404=VECTOR('',#8637,10.);
#1405=VECTOR('',#8638,10.);
#1406=VECTOR('',#8639,10.);
#1407=VECTOR('',#8640,10.);
#1408=VECTOR('',#8643,10.);
#1409=VECTOR('',#8644,10.);
#1410=VECTOR('',#8645,10.);
#1411=VECTOR('',#8648,10.);
#1412=VECTOR('',#8649,10.);
#1413=VECTOR('',#8650,10.);
#1414=VECTOR('',#8653,10.);
#1415=VECTOR('',#8654,10.);
#1416=VECTOR('',#8655,10.);
#1417=VECTOR('',#8658,10.);
#1418=VECTOR('',#8659,10.);
#1419=VECTOR('',#8660,10.);
#1420=VECTOR('',#8663,10.);
#1421=VECTOR('',#8664,10.);
#1422=VECTOR('',#8673,3.5);
#1423=CYLINDRICAL_SURFACE('',#6658,3.5);
#1424=CYLINDRICAL_SURFACE('',#6660,2.5);
#1425=CYLINDRICAL_SURFACE('',#6665,3.5);
#1426=CYLINDRICAL_SURFACE('',#6667,2.5);
#1427=CYLINDRICAL_SURFACE('',#6669,3.5);
#1428=CYLINDRICAL_SURFACE('',#6672,3.5);
#1429=CYLINDRICAL_SURFACE('',#6675,3.5);
#1430=CYLINDRICAL_SURFACE('',#6678,3.5);
#1431=CYLINDRICAL_SURFACE('',#6704,1.666);
#1432=CYLINDRICAL_SURFACE('',#6707,1.666);
#1433=CYLINDRICAL_SURFACE('',#6708,1.666);
#1434=CYLINDRICAL_SURFACE('',#6709,1.666);
#1435=CYLINDRICAL_SURFACE('',#6710,1.666);
#1436=CYLINDRICAL_SURFACE('',#6711,1.666);
#1437=CYLINDRICAL_SURFACE('',#6712,1.666);
#1438=CYLINDRICAL_SURFACE('',#6713,1.666);
#1439=CYLINDRICAL_SURFACE('',#6714,1.666);
#1440=CYLINDRICAL_SURFACE('',#6715,1.666);
#1441=CYLINDRICAL_SURFACE('',#6716,1.666);
#1442=CYLINDRICAL_SURFACE('',#6717,1.666);
#1443=CYLINDRICAL_SURFACE('',#6718,1.666);
#1444=CYLINDRICAL_SURFACE('',#6719,1.666);
#1445=CYLINDRICAL_SURFACE('',#6720,1.666);
#1446=CYLINDRICAL_SURFACE('',#6722,2.05475);
#1447=CYLINDRICAL_SURFACE('',#6724,2.05475);
#1448=CYLINDRICAL_SURFACE('',#6725,2.05475);
#1449=CYLINDRICAL_SURFACE('',#6726,2.05475);
#1450=CYLINDRICAL_SURFACE('',#6727,2.05475);
#1451=CYLINDRICAL_SURFACE('',#6728,2.05475);
#1452=CYLINDRICAL_SURFACE('',#6729,2.05475);
#1453=CYLINDRICAL_SURFACE('',#6730,2.05475);
#1454=CYLINDRICAL_SURFACE('',#6731,2.05475);
#1455=CYLINDRICAL_SURFACE('',#6732,2.05475);
#1456=CYLINDRICAL_SURFACE('',#6733,2.05475);
#1457=CYLINDRICAL_SURFACE('',#6734,2.05475);
#1458=CYLINDRICAL_SURFACE('',#6735,2.05475);
#1459=CYLINDRICAL_SURFACE('',#6736,2.05475);
#1460=CYLINDRICAL_SURFACE('',#6737,2.05475);
#1461=CYLINDRICAL_SURFACE('',#6738,2.05475);
#1462=CYLINDRICAL_SURFACE('',#6740,1.666);
#1463=CYLINDRICAL_SURFACE('',#6743,1.666);
#1464=CYLINDRICAL_SURFACE('',#6744,1.666);
#1465=CYLINDRICAL_SURFACE('',#6745,1.666);
#1466=CYLINDRICAL_SURFACE('',#6746,1.666);
#1467=CYLINDRICAL_SURFACE('',#6747,1.666);
#1468=CYLINDRICAL_SURFACE('',#6748,1.666);
#1469=CYLINDRICAL_SURFACE('',#6749,1.666);
#1470=CYLINDRICAL_SURFACE('',#6750,1.666);
#1471=CYLINDRICAL_SURFACE('',#6751,1.666);
#1472=CYLINDRICAL_SURFACE('',#6752,1.666);
#1473=CYLINDRICAL_SURFACE('',#6753,1.666);
#1474=CYLINDRICAL_SURFACE('',#6754,1.666);
#1475=CYLINDRICAL_SURFACE('',#6755,1.666);
#1476=CYLINDRICAL_SURFACE('',#6756,1.666);
#1477=CYLINDRICAL_SURFACE('',#6758,2.05475);
#1478=CYLINDRICAL_SURFACE('',#6760,2.05475);
#1479=CYLINDRICAL_SURFACE('',#6761,2.05475);
#1480=CYLINDRICAL_SURFACE('',#6762,2.05475);
#1481=CYLINDRICAL_SURFACE('',#6763,2.05475);
#1482=CYLINDRICAL_SURFACE('',#6764,2.05475);
#1483=CYLINDRICAL_SURFACE('',#6765,2.05475);
#1484=CYLINDRICAL_SURFACE('',#6766,2.05475);
#1485=CYLINDRICAL_SURFACE('',#6767,2.05475);
#1486=CYLINDRICAL_SURFACE('',#6768,2.05475);
#1487=CYLINDRICAL_SURFACE('',#6769,2.05475);
#1488=CYLINDRICAL_SURFACE('',#6770,2.05475);
#1489=CYLINDRICAL_SURFACE('',#6771,2.05475);
#1490=CYLINDRICAL_SURFACE('',#6772,2.05475);
#1491=CYLINDRICAL_SURFACE('',#6773,2.05475);
#1492=CYLINDRICAL_SURFACE('',#6774,2.05475);
#1493=CYLINDRICAL_SURFACE('',#6777,2.05475);
#1494=CYLINDRICAL_SURFACE('',#6778,1.666);
#1495=CYLINDRICAL_SURFACE('',#6780,2.05475);
#1496=CYLINDRICAL_SURFACE('',#6781,1.666);
#1497=CYLINDRICAL_SURFACE('',#6784,2.);
#1498=CYLINDRICAL_SURFACE('',#6787,4.);
#1499=CYLINDRICAL_SURFACE('',#6790,4.);
#1500=CYLINDRICAL_SURFACE('',#6828,2.5175);
#1501=CYLINDRICAL_SURFACE('',#6830,2.5175);
#1502=CYLINDRICAL_SURFACE('',#6831,2.5175);
#1503=CYLINDRICAL_SURFACE('',#6832,2.5175);
#1504=CYLINDRICAL_SURFACE('',#6833,2.5175);
#1505=CYLINDRICAL_SURFACE('',#6834,2.5175);
#1506=CYLINDRICAL_SURFACE('',#6835,2.5175);
#1507=CYLINDRICAL_SURFACE('',#6836,2.5175);
#1508=CYLINDRICAL_SURFACE('',#6837,2.5175);
#1509=CYLINDRICAL_SURFACE('',#6838,2.5175);
#1510=CYLINDRICAL_SURFACE('',#6840,3.0735);
#1511=CYLINDRICAL_SURFACE('',#6842,3.0735);
#1512=CYLINDRICAL_SURFACE('',#6843,3.0735);
#1513=CYLINDRICAL_SURFACE('',#6844,3.0735);
#1514=CYLINDRICAL_SURFACE('',#6845,3.0735);
#1515=CYLINDRICAL_SURFACE('',#6846,3.0735);
#1516=CYLINDRICAL_SURFACE('',#6847,3.0735);
#1517=CYLINDRICAL_SURFACE('',#6848,3.0735);
#1518=CYLINDRICAL_SURFACE('',#6849,3.0735);
#1519=CYLINDRICAL_SURFACE('',#6850,3.0735);
#1520=CYLINDRICAL_SURFACE('',#6852,26.9999999999999);
#1521=CYLINDRICAL_SURFACE('',#6855,2.);
#1522=CYLINDRICAL_SURFACE('',#6858,23.0000000000001);
#1523=CYLINDRICAL_SURFACE('',#6861,2.);
#1524=CYLINDRICAL_SURFACE('',#6864,3.0735);
#1525=CYLINDRICAL_SURFACE('',#6867,2.5175);
#1526=CYLINDRICAL_SURFACE('',#6868,3.);
#1527=CYLINDRICAL_SURFACE('',#6871,3.);
#1528=CYLINDRICAL_SURFACE('',#6874,5.);
#1529=CYLINDRICAL_SURFACE('',#6877,6.);
#1530=CYLINDRICAL_SURFACE('',#6879,10.);
#1531=CYLINDRICAL_SURFACE('',#6893,8.);
#1532=CYLINDRICAL_SURFACE('',#6896,6.);
#1533=CYLINDRICAL_SURFACE('',#6898,6.);
#1534=CYLINDRICAL_SURFACE('',#6901,3.);
#1535=CYLINDRICAL_SURFACE('',#6905,3.);
#1536=CYLINDRICAL_SURFACE('',#6927,2.);
#1537=CYLINDRICAL_SURFACE('',#6934,3.);
#1538=CYLINDRICAL_SURFACE('',#6939,5.);
#1539=CYLINDRICAL_SURFACE('',#6942,3.);
#1540=CYLINDRICAL_SURFACE('',#6945,3.);
#1541=CYLINDRICAL_SURFACE('',#6952,4.);
#1542=CYLINDRICAL_SURFACE('',#6957,7.);
#1543=CYLINDRICAL_SURFACE('',#6960,4.);
#1544=CYLINDRICAL_SURFACE('',#6963,3.);
#1545=CYLINDRICAL_SURFACE('',#6966,5.);
#1546=CYLINDRICAL_SURFACE('',#6977,2.);
#1547=CYLINDRICAL_SURFACE('',#6979,5.);
#1548=CYLINDRICAL_SURFACE('',#6983,4.);
#1549=CYLINDRICAL_SURFACE('',#6986,5.);
#1550=CYLINDRICAL_SURFACE('',#6992,4.);
#1551=CYLINDRICAL_SURFACE('',#6995,7.);
#1552=CYLINDRICAL_SURFACE('',#7001,4.);
#1553=CYLINDRICAL_SURFACE('',#7004,8.);
#1554=CYLINDRICAL_SURFACE('',#7015,3.);
#1555=CYLINDRICAL_SURFACE('',#7017,7.);
#1556=CYLINDRICAL_SURFACE('',#7021,1.5);
#1557=CYLINDRICAL_SURFACE('',#7028,2.);
#1558=CYLINDRICAL_SURFACE('',#7033,4.);
#1559=CYLINDRICAL_SURFACE('',#7036,2.);
#1560=CYLINDRICAL_SURFACE('',#7039,2.);
#1561=CYLINDRICAL_SURFACE('',#7042,4.);
#1562=CYLINDRICAL_SURFACE('',#7048,2.);
#1563=CYLINDRICAL_SURFACE('',#7051,4.);
#1564=CYLINDRICAL_SURFACE('',#7062,1.5);
#1565=CYLINDRICAL_SURFACE('',#7064,3.5);
#1566=CYLINDRICAL_SURFACE('',#7068,4.);
#1567=CYLINDRICAL_SURFACE('',#7071,14.);
#1568=CYLINDRICAL_SURFACE('',#7077,2.37175);
#1569=CYLINDRICAL_SURFACE('',#7079,2.37175);
#1570=CYLINDRICAL_SURFACE('',#7080,2.37175);
#1571=CYLINDRICAL_SURFACE('',#7081,2.37175);
#1572=CYLINDRICAL_SURFACE('',#7082,2.37175);
#1573=CYLINDRICAL_SURFACE('',#7083,2.37175);
#1574=CYLINDRICAL_SURFACE('',#7084,2.37175);
#1575=CYLINDRICAL_SURFACE('',#7085,2.37175);
#1576=CYLINDRICAL_SURFACE('',#7086,2.942);
#1577=CYLINDRICAL_SURFACE('',#7088,2.942);
#1578=CYLINDRICAL_SURFACE('',#7089,2.942);
#1579=CYLINDRICAL_SURFACE('',#7090,2.942);
#1580=CYLINDRICAL_SURFACE('',#7091,2.942);
#1581=CYLINDRICAL_SURFACE('',#7092,2.942);
#1582=CYLINDRICAL_SURFACE('',#7093,2.942);
#1583=CYLINDRICAL_SURFACE('',#7097,2.942);
#1584=CYLINDRICAL_SURFACE('',#7106,2.37175);
#1585=CYLINDRICAL_SURFACE('',#7110,6.);
#1586=CYLINDRICAL_SURFACE('',#7115,4.);
#1587=CYLINDRICAL_SURFACE('',#7118,1.954);
#1588=CYLINDRICAL_SURFACE('',#7120,1.954);
#1589=CYLINDRICAL_SURFACE('',#7121,1.954);
#1590=CYLINDRICAL_SURFACE('',#7122,1.954);
#1591=CYLINDRICAL_SURFACE('',#7123,1.954);
#1592=CYLINDRICAL_SURFACE('',#7124,1.954);
#1593=CYLINDRICAL_SURFACE('',#7125,1.954);
#1594=CYLINDRICAL_SURFACE('',#7126,1.954);
#1595=CYLINDRICAL_SURFACE('',#7127,1.954);
#1596=CYLINDRICAL_SURFACE('',#7128,1.954);
#1597=CYLINDRICAL_SURFACE('',#7129,1.954);
#1598=CYLINDRICAL_SURFACE('',#7130,1.954);
#1599=CYLINDRICAL_SURFACE('',#7131,1.954);
#1600=CYLINDRICAL_SURFACE('',#7132,1.5555);
#1601=CYLINDRICAL_SURFACE('',#7134,1.5555);
#1602=CYLINDRICAL_SURFACE('',#7135,1.5555);
#1603=CYLINDRICAL_SURFACE('',#7136,1.5555);
#1604=CYLINDRICAL_SURFACE('',#7137,1.5555);
#1605=CYLINDRICAL_SURFACE('',#7138,1.5555);
#1606=CYLINDRICAL_SURFACE('',#7139,1.5555);
#1607=CYLINDRICAL_SURFACE('',#7140,1.5555);
#1608=CYLINDRICAL_SURFACE('',#7141,1.5555);
#1609=CYLINDRICAL_SURFACE('',#7142,1.5555);
#1610=CYLINDRICAL_SURFACE('',#7143,1.5555);
#1611=CYLINDRICAL_SURFACE('',#7144,1.5555);
#1612=CYLINDRICAL_SURFACE('',#7145,1.5555);
#1613=CYLINDRICAL_SURFACE('',#7149,1.5555);
#1614=CYLINDRICAL_SURFACE('',#7151,1.954);
#1615=CYLINDRICAL_SURFACE('',#7161,3.5);
#1616=FACE_BOUND('',#2046,.T.);
#1617=FACE_BOUND('',#2050,.T.);
#1618=FACE_BOUND('',#2069,.T.);
#1619=FACE_BOUND('',#2070,.T.);
#1620=FACE_BOUND('',#2071,.T.);
#1621=FACE_BOUND('',#2073,.T.);
#1622=FACE_BOUND('',#2074,.T.);
#1623=FACE_BOUND('',#2079,.T.);
#1624=FACE_BOUND('',#2080,.T.);
#1625=FACE_BOUND('',#2081,.T.);
#1626=FACE_BOUND('',#2087,.T.);
#1627=FACE_BOUND('',#2088,.T.);
#1628=FACE_BOUND('',#2089,.T.);
#1629=FACE_BOUND('',#2090,.T.);
#1630=FACE_BOUND('',#2091,.T.);
#1631=FACE_BOUND('',#2092,.T.);
#1632=FACE_BOUND('',#2093,.T.);
#1633=FACE_BOUND('',#2094,.T.);
#1634=FACE_BOUND('',#2178,.T.);
#1635=FACE_BOUND('',#2183,.T.);
#1636=FACE_BOUND('',#2184,.T.);
#1637=FACE_BOUND('',#2186,.T.);
#1638=FACE_BOUND('',#2187,.T.);
#1639=FACE_BOUND('',#2191,.T.);
#1640=FACE_BOUND('',#2192,.T.);
#1641=FACE_BOUND('',#2208,.T.);
#1642=FACE_BOUND('',#2209,.T.);
#1643=FACE_BOUND('',#2211,.T.);
#1644=FACE_BOUND('',#2213,.T.);
#1645=FACE_BOUND('',#2215,.T.);
#1646=FACE_BOUND('',#2246,.T.);
#1647=FACE_BOUND('',#2254,.T.);
#1648=FACE_BOUND('',#2255,.T.);
#1649=FACE_BOUND('',#2256,.T.);
#1650=FACE_BOUND('',#2257,.T.);
#1651=FACE_BOUND('',#2258,.T.);
#1652=FACE_BOUND('',#2263,.T.);
#1653=FACE_BOUND('',#2264,.T.);
#1654=FACE_BOUND('',#2265,.T.);
#1655=FACE_BOUND('',#2266,.T.);
#1656=FACE_BOUND('',#2267,.T.);
#1657=FACE_BOUND('',#2291,.T.);
#1658=FACE_BOUND('',#2294,.T.);
#1659=FACE_BOUND('',#2300,.T.);
#1660=FACE_BOUND('',#2302,.T.);
#1661=FACE_BOUND('',#2305,.T.);
#1662=FACE_BOUND('',#2312,.T.);
#1663=FACE_BOUND('',#2314,.T.);
#1664=FACE_BOUND('',#2317,.T.);
#1665=FACE_BOUND('',#2325,.T.);
#1666=FACE_BOUND('',#2327,.T.);
#1667=FACE_BOUND('',#2337,.T.);
#1668=FACE_BOUND('',#2339,.T.);
#1669=FACE_BOUND('',#2343,.T.);
#1670=FACE_BOUND('',#2345,.T.);
#1671=FACE_BOUND('',#2349,.T.);
#1672=FACE_BOUND('',#2351,.T.);
#1673=FACE_BOUND('',#2360,.T.);
#1674=FACE_BOUND('',#2362,.T.);
#1675=FACE_BOUND('',#2365,.T.);
#1676=FACE_BOUND('',#2373,.T.);
#1677=FACE_BOUND('',#2375,.T.);
#1678=FACE_BOUND('',#2379,.T.);
#1679=FACE_BOUND('',#2381,.T.);
#1680=FACE_BOUND('',#2391,.T.);
#1681=FACE_BOUND('',#2393,.T.);
#1682=FACE_BOUND('',#2422,.T.);
#1683=FACE_BOUND('',#2425,.T.);
#1684=FACE_BOUND('',#2427,.T.);
#1685=FACE_BOUND('',#2469,.T.);
#1686=FACE_BOUND('',#2472,.T.);
#1687=FACE_OUTER_BOUND('',#2045,.T.);
#1688=FACE_OUTER_BOUND('',#2047,.T.);
#1689=FACE_OUTER_BOUND('',#2048,.T.);
#1690=FACE_OUTER_BOUND('',#2049,.T.);
#1691=FACE_OUTER_BOUND('',#2051,.T.);
#1692=FACE_OUTER_BOUND('',#2052,.T.);
#1693=FACE_OUTER_BOUND('',#2053,.T.);
#1694=FACE_OUTER_BOUND('',#2054,.T.);
#1695=FACE_OUTER_BOUND('',#2055,.T.);
#1696=FACE_OUTER_BOUND('',#2056,.T.);
#1697=FACE_OUTER_BOUND('',#2057,.T.);
#1698=FACE_OUTER_BOUND('',#2058,.T.);
#1699=FACE_OUTER_BOUND('',#2059,.T.);
#1700=FACE_OUTER_BOUND('',#2060,.T.);
#1701=FACE_OUTER_BOUND('',#2061,.T.);
#1702=FACE_OUTER_BOUND('',#2062,.T.);
#1703=FACE_OUTER_BOUND('',#2063,.T.);
#1704=FACE_OUTER_BOUND('',#2064,.T.);
#1705=FACE_OUTER_BOUND('',#2065,.T.);
#1706=FACE_OUTER_BOUND('',#2066,.T.);
#1707=FACE_OUTER_BOUND('',#2067,.T.);
#1708=FACE_OUTER_BOUND('',#2068,.T.);
#1709=FACE_OUTER_BOUND('',#2072,.T.);
#1710=FACE_OUTER_BOUND('',#2075,.T.);
#1711=FACE_OUTER_BOUND('',#2076,.T.);
#1712=FACE_OUTER_BOUND('',#2077,.T.);
#1713=FACE_OUTER_BOUND('',#2078,.T.);
#1714=FACE_OUTER_BOUND('',#2082,.T.);
#1715=FACE_OUTER_BOUND('',#2083,.T.);
#1716=FACE_OUTER_BOUND('',#2084,.T.);
#1717=FACE_OUTER_BOUND('',#2085,.T.);
#1718=FACE_OUTER_BOUND('',#2086,.T.);
#1719=FACE_OUTER_BOUND('',#2095,.T.);
#1720=FACE_OUTER_BOUND('',#2096,.T.);
#1721=FACE_OUTER_BOUND('',#2097,.T.);
#1722=FACE_OUTER_BOUND('',#2098,.T.);
#1723=FACE_OUTER_BOUND('',#2099,.T.);
#1724=FACE_OUTER_BOUND('',#2100,.T.);
#1725=FACE_OUTER_BOUND('',#2101,.T.);
#1726=FACE_OUTER_BOUND('',#2102,.T.);
#1727=FACE_OUTER_BOUND('',#2103,.T.);
#1728=FACE_OUTER_BOUND('',#2104,.T.);
#1729=FACE_OUTER_BOUND('',#2105,.T.);
#1730=FACE_OUTER_BOUND('',#2106,.T.);
#1731=FACE_OUTER_BOUND('',#2107,.T.);
#1732=FACE_OUTER_BOUND('',#2108,.T.);
#1733=FACE_OUTER_BOUND('',#2109,.T.);
#1734=FACE_OUTER_BOUND('',#2110,.T.);
#1735=FACE_OUTER_BOUND('',#2111,.T.);
#1736=FACE_OUTER_BOUND('',#2112,.T.);
#1737=FACE_OUTER_BOUND('',#2113,.T.);
#1738=FACE_OUTER_BOUND('',#2114,.T.);
#1739=FACE_OUTER_BOUND('',#2115,.T.);
#1740=FACE_OUTER_BOUND('',#2116,.T.);
#1741=FACE_OUTER_BOUND('',#2117,.T.);
#1742=FACE_OUTER_BOUND('',#2118,.T.);
#1743=FACE_OUTER_BOUND('',#2119,.T.);
#1744=FACE_OUTER_BOUND('',#2120,.T.);
#1745=FACE_OUTER_BOUND('',#2121,.T.);
#1746=FACE_OUTER_BOUND('',#2122,.T.);
#1747=FACE_OUTER_BOUND('',#2123,.T.);
#1748=FACE_OUTER_BOUND('',#2124,.T.);
#1749=FACE_OUTER_BOUND('',#2125,.T.);
#1750=FACE_OUTER_BOUND('',#2126,.T.);
#1751=FACE_OUTER_BOUND('',#2127,.T.);
#1752=FACE_OUTER_BOUND('',#2128,.T.);
#1753=FACE_OUTER_BOUND('',#2129,.T.);
#1754=FACE_OUTER_BOUND('',#2130,.T.);
#1755=FACE_OUTER_BOUND('',#2131,.T.);
#1756=FACE_OUTER_BOUND('',#2132,.T.);
#1757=FACE_OUTER_BOUND('',#2133,.T.);
#1758=FACE_OUTER_BOUND('',#2134,.T.);
#1759=FACE_OUTER_BOUND('',#2135,.T.);
#1760=FACE_OUTER_BOUND('',#2136,.T.);
#1761=FACE_OUTER_BOUND('',#2137,.T.);
#1762=FACE_OUTER_BOUND('',#2138,.T.);
#1763=FACE_OUTER_BOUND('',#2139,.T.);
#1764=FACE_OUTER_BOUND('',#2140,.T.);
#1765=FACE_OUTER_BOUND('',#2141,.T.);
#1766=FACE_OUTER_BOUND('',#2142,.T.);
#1767=FACE_OUTER_BOUND('',#2143,.T.);
#1768=FACE_OUTER_BOUND('',#2144,.T.);
#1769=FACE_OUTER_BOUND('',#2145,.T.);
#1770=FACE_OUTER_BOUND('',#2146,.T.);
#1771=FACE_OUTER_BOUND('',#2147,.T.);
#1772=FACE_OUTER_BOUND('',#2148,.T.);
#1773=FACE_OUTER_BOUND('',#2149,.T.);
#1774=FACE_OUTER_BOUND('',#2150,.T.);
#1775=FACE_OUTER_BOUND('',#2151,.T.);
#1776=FACE_OUTER_BOUND('',#2152,.T.);
#1777=FACE_OUTER_BOUND('',#2153,.T.);
#1778=FACE_OUTER_BOUND('',#2154,.T.);
#1779=FACE_OUTER_BOUND('',#2155,.T.);
#1780=FACE_OUTER_BOUND('',#2156,.T.);
#1781=FACE_OUTER_BOUND('',#2157,.T.);
#1782=FACE_OUTER_BOUND('',#2158,.T.);
#1783=FACE_OUTER_BOUND('',#2159,.T.);
#1784=FACE_OUTER_BOUND('',#2160,.T.);
#1785=FACE_OUTER_BOUND('',#2161,.T.);
#1786=FACE_OUTER_BOUND('',#2162,.T.);
#1787=FACE_OUTER_BOUND('',#2163,.T.);
#1788=FACE_OUTER_BOUND('',#2164,.T.);
#1789=FACE_OUTER_BOUND('',#2165,.T.);
#1790=FACE_OUTER_BOUND('',#2166,.T.);
#1791=FACE_OUTER_BOUND('',#2167,.T.);
#1792=FACE_OUTER_BOUND('',#2168,.T.);
#1793=FACE_OUTER_BOUND('',#2169,.T.);
#1794=FACE_OUTER_BOUND('',#2170,.T.);
#1795=FACE_OUTER_BOUND('',#2171,.T.);
#1796=FACE_OUTER_BOUND('',#2172,.T.);
#1797=FACE_OUTER_BOUND('',#2173,.T.);
#1798=FACE_OUTER_BOUND('',#2174,.T.);
#1799=FACE_OUTER_BOUND('',#2175,.T.);
#1800=FACE_OUTER_BOUND('',#2176,.T.);
#1801=FACE_OUTER_BOUND('',#2177,.T.);
#1802=FACE_OUTER_BOUND('',#2179,.T.);
#1803=FACE_OUTER_BOUND('',#2180,.T.);
#1804=FACE_OUTER_BOUND('',#2181,.T.);
#1805=FACE_OUTER_BOUND('',#2182,.T.);
#1806=FACE_OUTER_BOUND('',#2185,.T.);
#1807=FACE_OUTER_BOUND('',#2188,.T.);
#1808=FACE_OUTER_BOUND('',#2189,.T.);
#1809=FACE_OUTER_BOUND('',#2190,.T.);
#1810=FACE_OUTER_BOUND('',#2193,.T.);
#1811=FACE_OUTER_BOUND('',#2194,.T.);
#1812=FACE_OUTER_BOUND('',#2195,.T.);
#1813=FACE_OUTER_BOUND('',#2196,.T.);
#1814=FACE_OUTER_BOUND('',#2197,.T.);
#1815=FACE_OUTER_BOUND('',#2198,.T.);
#1816=FACE_OUTER_BOUND('',#2199,.T.);
#1817=FACE_OUTER_BOUND('',#2200,.T.);
#1818=FACE_OUTER_BOUND('',#2201,.T.);
#1819=FACE_OUTER_BOUND('',#2202,.T.);
#1820=FACE_OUTER_BOUND('',#2203,.T.);
#1821=FACE_OUTER_BOUND('',#2204,.T.);
#1822=FACE_OUTER_BOUND('',#2205,.T.);
#1823=FACE_OUTER_BOUND('',#2206,.T.);
#1824=FACE_OUTER_BOUND('',#2207,.T.);
#1825=FACE_OUTER_BOUND('',#2210,.T.);
#1826=FACE_OUTER_BOUND('',#2212,.T.);
#1827=FACE_OUTER_BOUND('',#2214,.T.);
#1828=FACE_OUTER_BOUND('',#2216,.T.);
#1829=FACE_OUTER_BOUND('',#2217,.T.);
#1830=FACE_OUTER_BOUND('',#2218,.T.);
#1831=FACE_OUTER_BOUND('',#2219,.T.);
#1832=FACE_OUTER_BOUND('',#2220,.T.);
#1833=FACE_OUTER_BOUND('',#2221,.T.);
#1834=FACE_OUTER_BOUND('',#2222,.T.);
#1835=FACE_OUTER_BOUND('',#2223,.T.);
#1836=FACE_OUTER_BOUND('',#2224,.T.);
#1837=FACE_OUTER_BOUND('',#2225,.T.);
#1838=FACE_OUTER_BOUND('',#2226,.T.);
#1839=FACE_OUTER_BOUND('',#2227,.T.);
#1840=FACE_OUTER_BOUND('',#2228,.T.);
#1841=FACE_OUTER_BOUND('',#2229,.T.);
#1842=FACE_OUTER_BOUND('',#2230,.T.);
#1843=FACE_OUTER_BOUND('',#2231,.T.);
#1844=FACE_OUTER_BOUND('',#2232,.T.);
#1845=FACE_OUTER_BOUND('',#2233,.T.);
#1846=FACE_OUTER_BOUND('',#2234,.T.);
#1847=FACE_OUTER_BOUND('',#2235,.T.);
#1848=FACE_OUTER_BOUND('',#2236,.T.);
#1849=FACE_OUTER_BOUND('',#2237,.T.);
#1850=FACE_OUTER_BOUND('',#2238,.T.);
#1851=FACE_OUTER_BOUND('',#2239,.T.);
#1852=FACE_OUTER_BOUND('',#2240,.T.);
#1853=FACE_OUTER_BOUND('',#2241,.T.);
#1854=FACE_OUTER_BOUND('',#2242,.T.);
#1855=FACE_OUTER_BOUND('',#2243,.T.);
#1856=FACE_OUTER_BOUND('',#2244,.T.);
#1857=FACE_OUTER_BOUND('',#2245,.T.);
#1858=FACE_OUTER_BOUND('',#2247,.T.);
#1859=FACE_OUTER_BOUND('',#2248,.T.);
#1860=FACE_OUTER_BOUND('',#2249,.T.);
#1861=FACE_OUTER_BOUND('',#2250,.T.);
#1862=FACE_OUTER_BOUND('',#2251,.T.);
#1863=FACE_OUTER_BOUND('',#2252,.T.);
#1864=FACE_OUTER_BOUND('',#2253,.T.);
#1865=FACE_OUTER_BOUND('',#2259,.T.);
#1866=FACE_OUTER_BOUND('',#2260,.T.);
#1867=FACE_OUTER_BOUND('',#2261,.T.);
#1868=FACE_OUTER_BOUND('',#2262,.T.);
#1869=FACE_OUTER_BOUND('',#2268,.T.);
#1870=FACE_OUTER_BOUND('',#2269,.T.);
#1871=FACE_OUTER_BOUND('',#2270,.T.);
#1872=FACE_OUTER_BOUND('',#2271,.T.);
#1873=FACE_OUTER_BOUND('',#2272,.T.);
#1874=FACE_OUTER_BOUND('',#2273,.T.);
#1875=FACE_OUTER_BOUND('',#2274,.T.);
#1876=FACE_OUTER_BOUND('',#2275,.T.);
#1877=FACE_OUTER_BOUND('',#2276,.T.);
#1878=FACE_OUTER_BOUND('',#2277,.T.);
#1879=FACE_OUTER_BOUND('',#2278,.T.);
#1880=FACE_OUTER_BOUND('',#2279,.T.);
#1881=FACE_OUTER_BOUND('',#2280,.T.);
#1882=FACE_OUTER_BOUND('',#2281,.T.);
#1883=FACE_OUTER_BOUND('',#2282,.T.);
#1884=FACE_OUTER_BOUND('',#2283,.T.);
#1885=FACE_OUTER_BOUND('',#2284,.T.);
#1886=FACE_OUTER_BOUND('',#2285,.T.);
#1887=FACE_OUTER_BOUND('',#2286,.T.);
#1888=FACE_OUTER_BOUND('',#2287,.T.);
#1889=FACE_OUTER_BOUND('',#2288,.T.);
#1890=FACE_OUTER_BOUND('',#2289,.T.);
#1891=FACE_OUTER_BOUND('',#2290,.T.);
#1892=FACE_OUTER_BOUND('',#2292,.T.);
#1893=FACE_OUTER_BOUND('',#2293,.T.);
#1894=FACE_OUTER_BOUND('',#2295,.T.);
#1895=FACE_OUTER_BOUND('',#2296,.T.);
#1896=FACE_OUTER_BOUND('',#2297,.T.);
#1897=FACE_OUTER_BOUND('',#2298,.T.);
#1898=FACE_OUTER_BOUND('',#2299,.T.);
#1899=FACE_OUTER_BOUND('',#2301,.T.);
#1900=FACE_OUTER_BOUND('',#2303,.T.);
#1901=FACE_OUTER_BOUND('',#2304,.T.);
#1902=FACE_OUTER_BOUND('',#2306,.T.);
#1903=FACE_OUTER_BOUND('',#2307,.T.);
#1904=FACE_OUTER_BOUND('',#2308,.T.);
#1905=FACE_OUTER_BOUND('',#2309,.T.);
#1906=FACE_OUTER_BOUND('',#2310,.T.);
#1907=FACE_OUTER_BOUND('',#2311,.T.);
#1908=FACE_OUTER_BOUND('',#2313,.T.);
#1909=FACE_OUTER_BOUND('',#2315,.T.);
#1910=FACE_OUTER_BOUND('',#2316,.T.);
#1911=FACE_OUTER_BOUND('',#2318,.T.);
#1912=FACE_OUTER_BOUND('',#2319,.T.);
#1913=FACE_OUTER_BOUND('',#2320,.T.);
#1914=FACE_OUTER_BOUND('',#2321,.T.);
#1915=FACE_OUTER_BOUND('',#2322,.T.);
#1916=FACE_OUTER_BOUND('',#2323,.T.);
#1917=FACE_OUTER_BOUND('',#2324,.T.);
#1918=FACE_OUTER_BOUND('',#2326,.T.);
#1919=FACE_OUTER_BOUND('',#2328,.T.);
#1920=FACE_OUTER_BOUND('',#2329,.T.);
#1921=FACE_OUTER_BOUND('',#2330,.T.);
#1922=FACE_OUTER_BOUND('',#2331,.T.);
#1923=FACE_OUTER_BOUND('',#2332,.T.);
#1924=FACE_OUTER_BOUND('',#2333,.T.);
#1925=FACE_OUTER_BOUND('',#2334,.T.);
#1926=FACE_OUTER_BOUND('',#2335,.T.);
#1927=FACE_OUTER_BOUND('',#2336,.T.);
#1928=FACE_OUTER_BOUND('',#2338,.T.);
#1929=FACE_OUTER_BOUND('',#2340,.T.);
#1930=FACE_OUTER_BOUND('',#2341,.T.);
#1931=FACE_OUTER_BOUND('',#2342,.T.);
#1932=FACE_OUTER_BOUND('',#2344,.T.);
#1933=FACE_OUTER_BOUND('',#2346,.T.);
#1934=FACE_OUTER_BOUND('',#2347,.T.);
#1935=FACE_OUTER_BOUND('',#2348,.T.);
#1936=FACE_OUTER_BOUND('',#2350,.T.);
#1937=FACE_OUTER_BOUND('',#2352,.T.);
#1938=FACE_OUTER_BOUND('',#2353,.T.);
#1939=FACE_OUTER_BOUND('',#2354,.T.);
#1940=FACE_OUTER_BOUND('',#2355,.T.);
#1941=FACE_OUTER_BOUND('',#2356,.T.);
#1942=FACE_OUTER_BOUND('',#2357,.T.);
#1943=FACE_OUTER_BOUND('',#2358,.T.);
#1944=FACE_OUTER_BOUND('',#2359,.T.);
#1945=FACE_OUTER_BOUND('',#2361,.T.);
#1946=FACE_OUTER_BOUND('',#2363,.T.);
#1947=FACE_OUTER_BOUND('',#2364,.T.);
#1948=FACE_OUTER_BOUND('',#2366,.T.);
#1949=FACE_OUTER_BOUND('',#2367,.T.);
#1950=FACE_OUTER_BOUND('',#2368,.T.);
#1951=FACE_OUTER_BOUND('',#2369,.T.);
#1952=FACE_OUTER_BOUND('',#2370,.T.);
#1953=FACE_OUTER_BOUND('',#2371,.T.);
#1954=FACE_OUTER_BOUND('',#2372,.T.);
#1955=FACE_OUTER_BOUND('',#2374,.T.);
#1956=FACE_OUTER_BOUND('',#2376,.T.);
#1957=FACE_OUTER_BOUND('',#2377,.T.);
#1958=FACE_OUTER_BOUND('',#2378,.T.);
#1959=FACE_OUTER_BOUND('',#2380,.T.);
#1960=FACE_OUTER_BOUND('',#2382,.T.);
#1961=FACE_OUTER_BOUND('',#2383,.T.);
#1962=FACE_OUTER_BOUND('',#2384,.T.);
#1963=FACE_OUTER_BOUND('',#2385,.T.);
#1964=FACE_OUTER_BOUND('',#2386,.T.);
#1965=FACE_OUTER_BOUND('',#2387,.T.);
#1966=FACE_OUTER_BOUND('',#2388,.T.);
#1967=FACE_OUTER_BOUND('',#2389,.T.);
#1968=FACE_OUTER_BOUND('',#2390,.T.);
#1969=FACE_OUTER_BOUND('',#2392,.T.);
#1970=FACE_OUTER_BOUND('',#2394,.T.);
#1971=FACE_OUTER_BOUND('',#2395,.T.);
#1972=FACE_OUTER_BOUND('',#2396,.T.);
#1973=FACE_OUTER_BOUND('',#2397,.T.);
#1974=FACE_OUTER_BOUND('',#2398,.T.);
#1975=FACE_OUTER_BOUND('',#2399,.T.);
#1976=FACE_OUTER_BOUND('',#2400,.T.);
#1977=FACE_OUTER_BOUND('',#2401,.T.);
#1978=FACE_OUTER_BOUND('',#2402,.T.);
#1979=FACE_OUTER_BOUND('',#2403,.T.);
#1980=FACE_OUTER_BOUND('',#2404,.T.);
#1981=FACE_OUTER_BOUND('',#2405,.T.);
#1982=FACE_OUTER_BOUND('',#2406,.T.);
#1983=FACE_OUTER_BOUND('',#2407,.T.);
#1984=FACE_OUTER_BOUND('',#2408,.T.);
#1985=FACE_OUTER_BOUND('',#2409,.T.);
#1986=FACE_OUTER_BOUND('',#2410,.T.);
#1987=FACE_OUTER_BOUND('',#2411,.T.);
#1988=FACE_OUTER_BOUND('',#2412,.T.);
#1989=FACE_OUTER_BOUND('',#2413,.T.);
#1990=FACE_OUTER_BOUND('',#2414,.T.);
#1991=FACE_OUTER_BOUND('',#2415,.T.);
#1992=FACE_OUTER_BOUND('',#2416,.T.);
#1993=FACE_OUTER_BOUND('',#2417,.T.);
#1994=FACE_OUTER_BOUND('',#2418,.T.);
#1995=FACE_OUTER_BOUND('',#2419,.T.);
#1996=FACE_OUTER_BOUND('',#2420,.T.);
#1997=FACE_OUTER_BOUND('',#2421,.T.);
#1998=FACE_OUTER_BOUND('',#2423,.T.);
#1999=FACE_OUTER_BOUND('',#2424,.T.);
#2000=FACE_OUTER_BOUND('',#2426,.T.);
#2001=FACE_OUTER_BOUND('',#2428,.T.);
#2002=FACE_OUTER_BOUND('',#2429,.T.);
#2003=FACE_OUTER_BOUND('',#2430,.T.);
#2004=FACE_OUTER_BOUND('',#2431,.T.);
#2005=FACE_OUTER_BOUND('',#2432,.T.);
#2006=FACE_OUTER_BOUND('',#2433,.T.);
#2007=FACE_OUTER_BOUND('',#2434,.T.);
#2008=FACE_OUTER_BOUND('',#2435,.T.);
#2009=FACE_OUTER_BOUND('',#2436,.T.);
#2010=FACE_OUTER_BOUND('',#2437,.T.);
#2011=FACE_OUTER_BOUND('',#2438,.T.);
#2012=FACE_OUTER_BOUND('',#2439,.T.);
#2013=FACE_OUTER_BOUND('',#2440,.T.);
#2014=FACE_OUTER_BOUND('',#2441,.T.);
#2015=FACE_OUTER_BOUND('',#2442,.T.);
#2016=FACE_OUTER_BOUND('',#2443,.T.);
#2017=FACE_OUTER_BOUND('',#2444,.T.);
#2018=FACE_OUTER_BOUND('',#2445,.T.);
#2019=FACE_OUTER_BOUND('',#2446,.T.);
#2020=FACE_OUTER_BOUND('',#2447,.T.);
#2021=FACE_OUTER_BOUND('',#2448,.T.);
#2022=FACE_OUTER_BOUND('',#2449,.T.);
#2023=FACE_OUTER_BOUND('',#2450,.T.);
#2024=FACE_OUTER_BOUND('',#2451,.T.);
#2025=FACE_OUTER_BOUND('',#2452,.T.);
#2026=FACE_OUTER_BOUND('',#2453,.T.);
#2027=FACE_OUTER_BOUND('',#2454,.T.);
#2028=FACE_OUTER_BOUND('',#2455,.T.);
#2029=FACE_OUTER_BOUND('',#2456,.T.);
#2030=FACE_OUTER_BOUND('',#2457,.T.);
#2031=FACE_OUTER_BOUND('',#2458,.T.);
#2032=FACE_OUTER_BOUND('',#2459,.T.);
#2033=FACE_OUTER_BOUND('',#2460,.T.);
#2034=FACE_OUTER_BOUND('',#2461,.T.);
#2035=FACE_OUTER_BOUND('',#2462,.T.);
#2036=FACE_OUTER_BOUND('',#2463,.T.);
#2037=FACE_OUTER_BOUND('',#2464,.T.);
#2038=FACE_OUTER_BOUND('',#2465,.T.);
#2039=FACE_OUTER_BOUND('',#2466,.T.);
#2040=FACE_OUTER_BOUND('',#2467,.T.);
#2041=FACE_OUTER_BOUND('',#2468,.T.);
#2042=FACE_OUTER_BOUND('',#2470,.T.);
#2043=FACE_OUTER_BOUND('',#2471,.T.);
#2044=FACE_OUTER_BOUND('',#2473,.T.);
#2045=EDGE_LOOP('',(#4115));
#2046=EDGE_LOOP('',(#4116));
#2047=EDGE_LOOP('',(#4117,#4118,#4119,#4120));
#2048=EDGE_LOOP('',(#4121,#4122,#4123,#4124));
#2049=EDGE_LOOP('',(#4125));
#2050=EDGE_LOOP('',(#4126));
#2051=EDGE_LOOP('',(#4127,#4128,#4129,#4130));
#2052=EDGE_LOOP('',(#4131,#4132,#4133,#4134));
#2053=EDGE_LOOP('',(#4135,#4136,#4137,#4138));
#2054=EDGE_LOOP('',(#4139,#4140,#4141,#4142));
#2055=EDGE_LOOP('',(#4143,#4144,#4145,#4146));
#2056=EDGE_LOOP('',(#4147,#4148,#4149,#4150));
#2057=EDGE_LOOP('',(#4151,#4152,#4153,#4154));
#2058=EDGE_LOOP('',(#4155,#4156,#4157,#4158));
#2059=EDGE_LOOP('',(#4159,#4160,#4161,#4162));
#2060=EDGE_LOOP('',(#4163,#4164,#4165,#4166));
#2061=EDGE_LOOP('',(#4167,#4168,#4169,#4170));
#2062=EDGE_LOOP('',(#4171,#4172,#4173,#4174));
#2063=EDGE_LOOP('',(#4175,#4176,#4177,#4178));
#2064=EDGE_LOOP('',(#4179,#4180,#4181,#4182));
#2065=EDGE_LOOP('',(#4183,#4184,#4185,#4186));
#2066=EDGE_LOOP('',(#4187,#4188,#4189,#4190));
#2067=EDGE_LOOP('',(#4191,#4192,#4193,#4194));
#2068=EDGE_LOOP('',(#4195,#4196,#4197,#4198));
#2069=EDGE_LOOP('',(#4199));
#2070=EDGE_LOOP('',(#4200));
#2071=EDGE_LOOP('',(#4201));
#2072=EDGE_LOOP('',(#4202,#4203,#4204,#4205));
#2073=EDGE_LOOP('',(#4206,#4207,#4208,#4209));
#2074=EDGE_LOOP('',(#4210,#4211,#4212,#4213));
#2075=EDGE_LOOP('',(#4214,#4215,#4216,#4217));
#2076=EDGE_LOOP('',(#4218,#4219,#4220,#4221));
#2077=EDGE_LOOP('',(#4222,#4223,#4224,#4225));
#2078=EDGE_LOOP('',(#4226,#4227,#4228,#4229));
#2079=EDGE_LOOP('',(#4230));
#2080=EDGE_LOOP('',(#4231));
#2081=EDGE_LOOP('',(#4232));
#2082=EDGE_LOOP('',(#4233,#4234,#4235,#4236));
#2083=EDGE_LOOP('',(#4237,#4238,#4239,#4240,#4241,#4242,#4243,#4244,#4245,
#4246,#4247,#4248));
#2084=EDGE_LOOP('',(#4249,#4250,#4251,#4252));
#2085=EDGE_LOOP('',(#4253,#4254,#4255,#4256,#4257,#4258,#4259,#4260,#4261,
#4262,#4263,#4264));
#2086=EDGE_LOOP('',(#4265,#4266,#4267,#4268));
#2087=EDGE_LOOP('',(#4269));
#2088=EDGE_LOOP('',(#4270));
#2089=EDGE_LOOP('',(#4271));
#2090=EDGE_LOOP('',(#4272));
#2091=EDGE_LOOP('',(#4273,#4274,#4275,#4276));
#2092=EDGE_LOOP('',(#4277,#4278,#4279,#4280));
#2093=EDGE_LOOP('',(#4281));
#2094=EDGE_LOOP('',(#4282));
#2095=EDGE_LOOP('',(#4283,#4284,#4285,#4286,#4287,#4288,#4289,#4290));
#2096=EDGE_LOOP('',(#4291,#4292,#4293,#4294));
#2097=EDGE_LOOP('',(#4295,#4296,#4297,#4298));
#2098=EDGE_LOOP('',(#4299,#4300,#4301,#4302));
#2099=EDGE_LOOP('',(#4303,#4304,#4305,#4306));
#2100=EDGE_LOOP('',(#4307,#4308,#4309,#4310));
#2101=EDGE_LOOP('',(#4311,#4312,#4313,#4314));
#2102=EDGE_LOOP('',(#4315,#4316,#4317,#4318));
#2103=EDGE_LOOP('',(#4319,#4320,#4321,#4322));
#2104=EDGE_LOOP('',(#4323,#4324,#4325,#4326));
#2105=EDGE_LOOP('',(#4327,#4328,#4329,#4330));
#2106=EDGE_LOOP('',(#4331,#4332,#4333,#4334));
#2107=EDGE_LOOP('',(#4335,#4336,#4337,#4338));
#2108=EDGE_LOOP('',(#4339,#4340,#4341,#4342));
#2109=EDGE_LOOP('',(#4343,#4344,#4345,#4346));
#2110=EDGE_LOOP('',(#4347,#4348,#4349,#4350));
#2111=EDGE_LOOP('',(#4351,#4352,#4353,#4354));
#2112=EDGE_LOOP('',(#4355,#4356,#4357,#4358));
#2113=EDGE_LOOP('',(#4359,#4360,#4361,#4362));
#2114=EDGE_LOOP('',(#4363,#4364,#4365,#4366));
#2115=EDGE_LOOP('',(#4367,#4368,#4369,#4370));
#2116=EDGE_LOOP('',(#4371,#4372,#4373,#4374));
#2117=EDGE_LOOP('',(#4375,#4376,#4377,#4378));
#2118=EDGE_LOOP('',(#4379,#4380,#4381,#4382));
#2119=EDGE_LOOP('',(#4383,#4384,#4385,#4386));
#2120=EDGE_LOOP('',(#4387,#4388,#4389,#4390));
#2121=EDGE_LOOP('',(#4391,#4392,#4393,#4394));
#2122=EDGE_LOOP('',(#4395,#4396,#4397,#4398));
#2123=EDGE_LOOP('',(#4399,#4400,#4401,#4402));
#2124=EDGE_LOOP('',(#4403,#4404,#4405,#4406));
#2125=EDGE_LOOP('',(#4407,#4408,#4409,#4410));
#2126=EDGE_LOOP('',(#4411,#4412,#4413,#4414,#4415,#4416,#4417,#4418));
#2127=EDGE_LOOP('',(#4419,#4420,#4421,#4422));
#2128=EDGE_LOOP('',(#4423,#4424,#4425,#4426));
#2129=EDGE_LOOP('',(#4427,#4428,#4429,#4430));
#2130=EDGE_LOOP('',(#4431,#4432,#4433,#4434));
#2131=EDGE_LOOP('',(#4435,#4436,#4437,#4438));
#2132=EDGE_LOOP('',(#4439,#4440,#4441,#4442));
#2133=EDGE_LOOP('',(#4443,#4444,#4445,#4446));
#2134=EDGE_LOOP('',(#4447,#4448,#4449,#4450));
#2135=EDGE_LOOP('',(#4451,#4452,#4453,#4454));
#2136=EDGE_LOOP('',(#4455,#4456,#4457,#4458));
#2137=EDGE_LOOP('',(#4459,#4460,#4461,#4462));
#2138=EDGE_LOOP('',(#4463,#4464,#4465,#4466));
#2139=EDGE_LOOP('',(#4467,#4468,#4469,#4470));
#2140=EDGE_LOOP('',(#4471,#4472,#4473,#4474));
#2141=EDGE_LOOP('',(#4475,#4476,#4477,#4478));
#2142=EDGE_LOOP('',(#4479,#4480,#4481,#4482));
#2143=EDGE_LOOP('',(#4483,#4484,#4485,#4486));
#2144=EDGE_LOOP('',(#4487,#4488,#4489,#4490));
#2145=EDGE_LOOP('',(#4491,#4492,#4493,#4494));
#2146=EDGE_LOOP('',(#4495,#4496,#4497,#4498));
#2147=EDGE_LOOP('',(#4499,#4500,#4501,#4502));
#2148=EDGE_LOOP('',(#4503,#4504,#4505,#4506));
#2149=EDGE_LOOP('',(#4507,#4508,#4509,#4510));
#2150=EDGE_LOOP('',(#4511,#4512,#4513,#4514));
#2151=EDGE_LOOP('',(#4515,#4516,#4517,#4518));
#2152=EDGE_LOOP('',(#4519,#4520,#4521,#4522));
#2153=EDGE_LOOP('',(#4523,#4524,#4525,#4526));
#2154=EDGE_LOOP('',(#4527,#4528,#4529,#4530));
#2155=EDGE_LOOP('',(#4531,#4532,#4533,#4534));
#2156=EDGE_LOOP('',(#4535,#4536,#4537,#4538));
#2157=EDGE_LOOP('',(#4539,#4540,#4541,#4542));
#2158=EDGE_LOOP('',(#4543,#4544,#4545,#4546));
#2159=EDGE_LOOP('',(#4547,#4548,#4549,#4550,#4551,#4552,#4553,#4554,#4555,
#4556,#4557,#4558,#4559,#4560,#4561,#4562,#4563,#4564,#4565,#4566,#4567,
#4568,#4569,#4570,#4571,#4572,#4573,#4574,#4575,#4576,#4577,#4578,#4579,
#4580,#4581,#4582));
#2160=EDGE_LOOP('',(#4583,#4584,#4585,#4586,#4587,#4588,#4589,#4590,#4591,
#4592,#4593,#4594,#4595,#4596,#4597,#4598,#4599,#4600,#4601,#4602,#4603,
#4604,#4605,#4606,#4607,#4608,#4609,#4610,#4611,#4612,#4613,#4614,#4615,
#4616,#4617));
#2161=EDGE_LOOP('',(#4618,#4619,#4620,#4621));
#2162=EDGE_LOOP('',(#4622,#4623,#4624,#4625));
#2163=EDGE_LOOP('',(#4626,#4627,#4628,#4629));
#2164=EDGE_LOOP('',(#4630,#4631,#4632,#4633,#4634,#4635,#4636,#4637,#4638,
#4639,#4640,#4641,#4642,#4643,#4644,#4645,#4646,#4647,#4648,#4649,#4650,
#4651,#4652,#4653,#4654,#4655,#4656,#4657,#4658,#4659,#4660,#4661,#4662,
#4663,#4664,#4665));
#2165=EDGE_LOOP('',(#4666,#4667,#4668,#4669,#4670,#4671,#4672,#4673,#4674,
#4675,#4676,#4677,#4678,#4679,#4680,#4681,#4682,#4683,#4684,#4685,#4686,
#4687,#4688,#4689,#4690,#4691,#4692,#4693,#4694,#4695,#4696,#4697,#4698,
#4699,#4700));
#2166=EDGE_LOOP('',(#4701,#4702,#4703,#4704));
#2167=EDGE_LOOP('',(#4705));
#2168=EDGE_LOOP('',(#4706));
#2169=EDGE_LOOP('',(#4707,#4708,#4709,#4710));
#2170=EDGE_LOOP('',(#4711,#4712,#4713,#4714));
#2171=EDGE_LOOP('',(#4715,#4716,#4717,#4718));
#2172=EDGE_LOOP('',(#4719,#4720,#4721,#4722));
#2173=EDGE_LOOP('',(#4723,#4724,#4725,#4726));
#2174=EDGE_LOOP('',(#4727,#4728,#4729,#4730));
#2175=EDGE_LOOP('',(#4731,#4732,#4733,#4734));
#2176=EDGE_LOOP('',(#4735,#4736,#4737,#4738));
#2177=EDGE_LOOP('',(#4739,#4740,#4741,#4742));
#2178=EDGE_LOOP('',(#4743));
#2179=EDGE_LOOP('',(#4744,#4745,#4746,#4747));
#2180=EDGE_LOOP('',(#4748,#4749,#4750,#4751));
#2181=EDGE_LOOP('',(#4752,#4753,#4754,#4755));
#2182=EDGE_LOOP('',(#4756,#4757,#4758,#4759,#4760,#4761,#4762,#4763,#4764,
#4765,#4766,#4767));
#2183=EDGE_LOOP('',(#4768,#4769,#4770,#4771));
#2184=EDGE_LOOP('',(#4772,#4773,#4774,#4775));
#2185=EDGE_LOOP('',(#4776,#4777,#4778,#4779,#4780,#4781,#4782,#4783));
#2186=EDGE_LOOP('',(#4784));
#2187=EDGE_LOOP('',(#4785));
#2188=EDGE_LOOP('',(#4786,#4787,#4788,#4789));
#2189=EDGE_LOOP('',(#4790,#4791,#4792,#4793));
#2190=EDGE_LOOP('',(#4794,#4795,#4796,#4797,#4798,#4799,#4800,#4801,#4802,
#4803,#4804,#4805,#4806,#4807,#4808,#4809));
#2191=EDGE_LOOP('',(#4810));
#2192=EDGE_LOOP('',(#4811));
#2193=EDGE_LOOP('',(#4812,#4813,#4814,#4815));
#2194=EDGE_LOOP('',(#4816,#4817,#4818,#4819));
#2195=EDGE_LOOP('',(#4820,#4821,#4822,#4823));
#2196=EDGE_LOOP('',(#4824,#4825,#4826,#4827));
#2197=EDGE_LOOP('',(#4828,#4829,#4830,#4831));
#2198=EDGE_LOOP('',(#4832,#4833,#4834,#4835));
#2199=EDGE_LOOP('',(#4836,#4837,#4838,#4839));
#2200=EDGE_LOOP('',(#4840,#4841,#4842,#4843));
#2201=EDGE_LOOP('',(#4844,#4845,#4846,#4847,#4848,#4849,#4850,#4851));
#2202=EDGE_LOOP('',(#4852,#4853,#4854,#4855));
#2203=EDGE_LOOP('',(#4856,#4857,#4858,#4859));
#2204=EDGE_LOOP('',(#4860,#4861,#4862,#4863));
#2205=EDGE_LOOP('',(#4864,#4865,#4866,#4867,#4868,#4869,#4870,#4871));
#2206=EDGE_LOOP('',(#4872,#4873,#4874,#4875));
#2207=EDGE_LOOP('',(#4876,#4877,#4878,#4879));
#2208=EDGE_LOOP('',(#4880,#4881,#4882,#4883));
#2209=EDGE_LOOP('',(#4884,#4885,#4886,#4887));
#2210=EDGE_LOOP('',(#4888,#4889,#4890,#4891));
#2211=EDGE_LOOP('',(#4892,#4893,#4894,#4895));
#2212=EDGE_LOOP('',(#4896,#4897,#4898,#4899));
#2213=EDGE_LOOP('',(#4900,#4901,#4902,#4903));
#2214=EDGE_LOOP('',(#4904,#4905,#4906,#4907,#4908,#4909,#4910,#4911,#4912,
#4913,#4914,#4915));
#2215=EDGE_LOOP('',(#4916));
#2216=EDGE_LOOP('',(#4917,#4918,#4919,#4920));
#2217=EDGE_LOOP('',(#4921,#4922,#4923,#4924));
#2218=EDGE_LOOP('',(#4925,#4926,#4927,#4928));
#2219=EDGE_LOOP('',(#4929,#4930,#4931,#4932));
#2220=EDGE_LOOP('',(#4933,#4934,#4935,#4936));
#2221=EDGE_LOOP('',(#4937,#4938,#4939,#4940));
#2222=EDGE_LOOP('',(#4941,#4942,#4943,#4944));
#2223=EDGE_LOOP('',(#4945,#4946,#4947,#4948));
#2224=EDGE_LOOP('',(#4949,#4950,#4951,#4952));
#2225=EDGE_LOOP('',(#4953,#4954,#4955,#4956));
#2226=EDGE_LOOP('',(#4957,#4958,#4959,#4960));
#2227=EDGE_LOOP('',(#4961,#4962,#4963,#4964));
#2228=EDGE_LOOP('',(#4965,#4966,#4967,#4968));
#2229=EDGE_LOOP('',(#4969,#4970,#4971,#4972));
#2230=EDGE_LOOP('',(#4973,#4974,#4975,#4976));
#2231=EDGE_LOOP('',(#4977,#4978,#4979,#4980));
#2232=EDGE_LOOP('',(#4981,#4982,#4983,#4984));
#2233=EDGE_LOOP('',(#4985,#4986,#4987,#4988));
#2234=EDGE_LOOP('',(#4989,#4990,#4991,#4992));
#2235=EDGE_LOOP('',(#4993,#4994,#4995,#4996));
#2236=EDGE_LOOP('',(#4997,#4998,#4999,#5000));
#2237=EDGE_LOOP('',(#5001,#5002,#5003,#5004));
#2238=EDGE_LOOP('',(#5005,#5006,#5007,#5008));
#2239=EDGE_LOOP('',(#5009,#5010,#5011,#5012));
#2240=EDGE_LOOP('',(#5013,#5014,#5015,#5016));
#2241=EDGE_LOOP('',(#5017,#5018,#5019,#5020));
#2242=EDGE_LOOP('',(#5021,#5022,#5023,#5024));
#2243=EDGE_LOOP('',(#5025,#5026,#5027,#5028,#5029,#5030,#5031,#5032,#5033,
#5034,#5035,#5036,#5037,#5038,#5039,#5040,#5041,#5042,#5043,#5044,#5045,
#5046,#5047,#5048));
#2244=EDGE_LOOP('',(#5049,#5050,#5051,#5052,#5053,#5054,#5055,#5056,#5057,
#5058,#5059,#5060,#5061,#5062,#5063,#5064,#5065,#5066,#5067,#5068,#5069,
#5070,#5071,#5072));
#2245=EDGE_LOOP('',(#5073));
#2246=EDGE_LOOP('',(#5074,#5075,#5076,#5077));
#2247=EDGE_LOOP('',(#5078,#5079,#5080,#5081));
#2248=EDGE_LOOP('',(#5082,#5083,#5084,#5085));
#2249=EDGE_LOOP('',(#5086,#5087,#5088,#5089));
#2250=EDGE_LOOP('',(#5090,#5091,#5092,#5093));
#2251=EDGE_LOOP('',(#5094,#5095,#5096,#5097));
#2252=EDGE_LOOP('',(#5098,#5099,#5100,#5101));
#2253=EDGE_LOOP('',(#5102,#5103,#5104,#5105,#5106,#5107,#5108,#5109,#5110,
#5111));
#2254=EDGE_LOOP('',(#5112,#5113,#5114,#5115));
#2255=EDGE_LOOP('',(#5116));
#2256=EDGE_LOOP('',(#5117));
#2257=EDGE_LOOP('',(#5118));
#2258=EDGE_LOOP('',(#5119));
#2259=EDGE_LOOP('',(#5120,#5121,#5122,#5123));
#2260=EDGE_LOOP('',(#5124,#5125,#5126,#5127));
#2261=EDGE_LOOP('',(#5128,#5129,#5130,#5131));
#2262=EDGE_LOOP('',(#5132,#5133,#5134,#5135,#5136,#5137,#5138,#5139,#5140,
#5141));
#2263=EDGE_LOOP('',(#5142,#5143,#5144,#5145));
#2264=EDGE_LOOP('',(#5146,#5147,#5148,#5149));
#2265=EDGE_LOOP('',(#5150));
#2266=EDGE_LOOP('',(#5151));
#2267=EDGE_LOOP('',(#5152));
#2268=EDGE_LOOP('',(#5153,#5154,#5155,#5156));
#2269=EDGE_LOOP('',(#5157,#5158,#5159,#5160));
#2270=EDGE_LOOP('',(#5161,#5162,#5163,#5164));
#2271=EDGE_LOOP('',(#5165,#5166,#5167,#5168));
#2272=EDGE_LOOP('',(#5169,#5170,#5171,#5172));
#2273=EDGE_LOOP('',(#5173,#5174,#5175,#5176));
#2274=EDGE_LOOP('',(#5177,#5178,#5179,#5180));
#2275=EDGE_LOOP('',(#5181,#5182,#5183,#5184));
#2276=EDGE_LOOP('',(#5185,#5186,#5187,#5188));
#2277=EDGE_LOOP('',(#5189,#5190,#5191,#5192));
#2278=EDGE_LOOP('',(#5193,#5194,#5195,#5196));
#2279=EDGE_LOOP('',(#5197,#5198,#5199,#5200));
#2280=EDGE_LOOP('',(#5201,#5202,#5203,#5204));
#2281=EDGE_LOOP('',(#5205,#5206,#5207,#5208,#5209,#5210));
#2282=EDGE_LOOP('',(#5211,#5212,#5213,#5214));
#2283=EDGE_LOOP('',(#5215,#5216,#5217,#5218,#5219,#5220));
#2284=EDGE_LOOP('',(#5221,#5222,#5223,#5224));
#2285=EDGE_LOOP('',(#5225,#5226,#5227,#5228));
#2286=EDGE_LOOP('',(#5229,#5230,#5231,#5232));
#2287=EDGE_LOOP('',(#5233,#5234,#5235,#5236));
#2288=EDGE_LOOP('',(#5237,#5238,#5239,#5240));
#2289=EDGE_LOOP('',(#5241,#5242,#5243,#5244));
#2290=EDGE_LOOP('',(#5245,#5246,#5247,#5248,#5249,#5250,#5251,#5252,#5253,
#5254));
#2291=EDGE_LOOP('',(#5255,#5256,#5257,#5258));
#2292=EDGE_LOOP('',(#5259,#5260,#5261,#5262));
#2293=EDGE_LOOP('',(#5263,#5264,#5265,#5266,#5267,#5268,#5269,#5270,#5271,
#5272));
#2294=EDGE_LOOP('',(#5273,#5274,#5275,#5276));
#2295=EDGE_LOOP('',(#5277,#5278,#5279,#5280));
#2296=EDGE_LOOP('',(#5281,#5282,#5283,#5284));
#2297=EDGE_LOOP('',(#5285,#5286,#5287,#5288));
#2298=EDGE_LOOP('',(#5289,#5290,#5291,#5292));
#2299=EDGE_LOOP('',(#5293));
#2300=EDGE_LOOP('',(#5294));
#2301=EDGE_LOOP('',(#5295));
#2302=EDGE_LOOP('',(#5296));
#2303=EDGE_LOOP('',(#5297,#5298,#5299,#5300));
#2304=EDGE_LOOP('',(#5301));
#2305=EDGE_LOOP('',(#5302));
#2306=EDGE_LOOP('',(#5303,#5304,#5305,#5306));
#2307=EDGE_LOOP('',(#5307));
#2308=EDGE_LOOP('',(#5308,#5309,#5310,#5311));
#2309=EDGE_LOOP('',(#5312));
#2310=EDGE_LOOP('',(#5313,#5314,#5315,#5316));
#2311=EDGE_LOOP('',(#5317));
#2312=EDGE_LOOP('',(#5318));
#2313=EDGE_LOOP('',(#5319));
#2314=EDGE_LOOP('',(#5320));
#2315=EDGE_LOOP('',(#5321,#5322,#5323,#5324));
#2316=EDGE_LOOP('',(#5325));
#2317=EDGE_LOOP('',(#5326));
#2318=EDGE_LOOP('',(#5327,#5328,#5329,#5330));
#2319=EDGE_LOOP('',(#5331));
#2320=EDGE_LOOP('',(#5332,#5333,#5334,#5335));
#2321=EDGE_LOOP('',(#5336));
#2322=EDGE_LOOP('',(#5337,#5338,#5339,#5340));
#2323=EDGE_LOOP('',(#5341,#5342,#5343,#5344));
#2324=EDGE_LOOP('',(#5345));
#2325=EDGE_LOOP('',(#5346));
#2326=EDGE_LOOP('',(#5347));
#2327=EDGE_LOOP('',(#5348));
#2328=EDGE_LOOP('',(#5349,#5350,#5351,#5352));
#2329=EDGE_LOOP('',(#5353,#5354,#5355,#5356));
#2330=EDGE_LOOP('',(#5357,#5358,#5359,#5360));
#2331=EDGE_LOOP('',(#5361,#5362,#5363,#5364));
#2332=EDGE_LOOP('',(#5365,#5366,#5367,#5368));
#2333=EDGE_LOOP('',(#5369,#5370,#5371,#5372));
#2334=EDGE_LOOP('',(#5373,#5374,#5375,#5376));
#2335=EDGE_LOOP('',(#5377,#5378,#5379,#5380));
#2336=EDGE_LOOP('',(#5381));
#2337=EDGE_LOOP('',(#5382));
#2338=EDGE_LOOP('',(#5383));
#2339=EDGE_LOOP('',(#5384));
#2340=EDGE_LOOP('',(#5385,#5386,#5387,#5388));
#2341=EDGE_LOOP('',(#5389,#5390,#5391,#5392));
#2342=EDGE_LOOP('',(#5393));
#2343=EDGE_LOOP('',(#5394));
#2344=EDGE_LOOP('',(#5395));
#2345=EDGE_LOOP('',(#5396));
#2346=EDGE_LOOP('',(#5397,#5398,#5399,#5400));
#2347=EDGE_LOOP('',(#5401,#5402,#5403,#5404));
#2348=EDGE_LOOP('',(#5405));
#2349=EDGE_LOOP('',(#5406));
#2350=EDGE_LOOP('',(#5407));
#2351=EDGE_LOOP('',(#5408));
#2352=EDGE_LOOP('',(#5409,#5410,#5411,#5412));
#2353=EDGE_LOOP('',(#5413,#5414,#5415,#5416));
#2354=EDGE_LOOP('',(#5417,#5418,#5419,#5420));
#2355=EDGE_LOOP('',(#5421,#5422,#5423,#5424));
#2356=EDGE_LOOP('',(#5425,#5426,#5427,#5428));
#2357=EDGE_LOOP('',(#5429,#5430,#5431,#5432));
#2358=EDGE_LOOP('',(#5433,#5434,#5435,#5436));
#2359=EDGE_LOOP('',(#5437));
#2360=EDGE_LOOP('',(#5438));
#2361=EDGE_LOOP('',(#5439));
#2362=EDGE_LOOP('',(#5440));
#2363=EDGE_LOOP('',(#5441,#5442,#5443,#5444));
#2364=EDGE_LOOP('',(#5445));
#2365=EDGE_LOOP('',(#5446));
#2366=EDGE_LOOP('',(#5447,#5448,#5449,#5450));
#2367=EDGE_LOOP('',(#5451));
#2368=EDGE_LOOP('',(#5452,#5453,#5454,#5455));
#2369=EDGE_LOOP('',(#5456));
#2370=EDGE_LOOP('',(#5457,#5458,#5459,#5460));
#2371=EDGE_LOOP('',(#5461,#5462,#5463,#5464));
#2372=EDGE_LOOP('',(#5465));
#2373=EDGE_LOOP('',(#5466));
#2374=EDGE_LOOP('',(#5467));
#2375=EDGE_LOOP('',(#5468));
#2376=EDGE_LOOP('',(#5469,#5470,#5471,#5472));
#2377=EDGE_LOOP('',(#5473,#5474,#5475,#5476));
#2378=EDGE_LOOP('',(#5477));
#2379=EDGE_LOOP('',(#5478));
#2380=EDGE_LOOP('',(#5479));
#2381=EDGE_LOOP('',(#5480));
#2382=EDGE_LOOP('',(#5481,#5482,#5483,#5484));
#2383=EDGE_LOOP('',(#5485,#5486,#5487,#5488));
#2384=EDGE_LOOP('',(#5489,#5490,#5491,#5492));
#2385=EDGE_LOOP('',(#5493,#5494,#5495,#5496));
#2386=EDGE_LOOP('',(#5497,#5498,#5499,#5500));
#2387=EDGE_LOOP('',(#5501,#5502,#5503,#5504));
#2388=EDGE_LOOP('',(#5505,#5506,#5507,#5508));
#2389=EDGE_LOOP('',(#5509,#5510,#5511,#5512));
#2390=EDGE_LOOP('',(#5513));
#2391=EDGE_LOOP('',(#5514));
#2392=EDGE_LOOP('',(#5515));
#2393=EDGE_LOOP('',(#5516));
#2394=EDGE_LOOP('',(#5517,#5518,#5519,#5520));
#2395=EDGE_LOOP('',(#5521,#5522,#5523,#5524));
#2396=EDGE_LOOP('',(#5525,#5526,#5527,#5528));
#2397=EDGE_LOOP('',(#5529,#5530,#5531,#5532));
#2398=EDGE_LOOP('',(#5533,#5534,#5535,#5536));
#2399=EDGE_LOOP('',(#5537,#5538,#5539,#5540));
#2400=EDGE_LOOP('',(#5541,#5542,#5543,#5544));
#2401=EDGE_LOOP('',(#5545,#5546,#5547,#5548));
#2402=EDGE_LOOP('',(#5549,#5550,#5551,#5552));
#2403=EDGE_LOOP('',(#5553,#5554,#5555,#5556));
#2404=EDGE_LOOP('',(#5557,#5558,#5559,#5560));
#2405=EDGE_LOOP('',(#5561,#5562,#5563,#5564));
#2406=EDGE_LOOP('',(#5565,#5566,#5567,#5568));
#2407=EDGE_LOOP('',(#5569,#5570,#5571,#5572));
#2408=EDGE_LOOP('',(#5573,#5574,#5575,#5576));
#2409=EDGE_LOOP('',(#5577,#5578,#5579,#5580,#5581,#5582,#5583,#5584));
#2410=EDGE_LOOP('',(#5585,#5586,#5587,#5588,#5589,#5590,#5591,#5592,#5593,
#5594,#5595,#5596,#5597,#5598,#5599,#5600,#5601,#5602,#5603,#5604));
#2411=EDGE_LOOP('',(#5605,#5606,#5607,#5608));
#2412=EDGE_LOOP('',(#5609,#5610,#5611,#5612));
#2413=EDGE_LOOP('',(#5613,#5614,#5615,#5616));
#2414=EDGE_LOOP('',(#5617,#5618,#5619,#5620));
#2415=EDGE_LOOP('',(#5621,#5622,#5623,#5624));
#2416=EDGE_LOOP('',(#5625,#5626,#5627,#5628));
#2417=EDGE_LOOP('',(#5629,#5630,#5631,#5632));
#2418=EDGE_LOOP('',(#5633,#5634,#5635,#5636,#5637,#5638));
#2419=EDGE_LOOP('',(#5639,#5640,#5641,#5642,#5643,#5644,#5645,#5646,#5647,
#5648,#5649,#5650,#5651,#5652,#5653,#5654,#5655,#5656,#5657));
#2420=EDGE_LOOP('',(#5658,#5659,#5660,#5661));
#2421=EDGE_LOOP('',(#5662));
#2422=EDGE_LOOP('',(#5663));
#2423=EDGE_LOOP('',(#5664,#5665,#5666,#5667));
#2424=EDGE_LOOP('',(#5668));
#2425=EDGE_LOOP('',(#5669,#5670,#5671,#5672,#5673,#5674));
#2426=EDGE_LOOP('',(#5675));
#2427=EDGE_LOOP('',(#5676,#5677,#5678,#5679));
#2428=EDGE_LOOP('',(#5680,#5681,#5682,#5683));
#2429=EDGE_LOOP('',(#5684));
#2430=EDGE_LOOP('',(#5685,#5686,#5687,#5688));
#2431=EDGE_LOOP('',(#5689,#5690,#5691,#5692));
#2432=EDGE_LOOP('',(#5693,#5694,#5695,#5696));
#2433=EDGE_LOOP('',(#5697,#5698,#5699,#5700));
#2434=EDGE_LOOP('',(#5701,#5702,#5703,#5704));
#2435=EDGE_LOOP('',(#5705,#5706,#5707,#5708));
#2436=EDGE_LOOP('',(#5709,#5710,#5711,#5712));
#2437=EDGE_LOOP('',(#5713,#5714,#5715,#5716));
#2438=EDGE_LOOP('',(#5717,#5718,#5719,#5720));
#2439=EDGE_LOOP('',(#5721,#5722,#5723,#5724));
#2440=EDGE_LOOP('',(#5725,#5726,#5727,#5728));
#2441=EDGE_LOOP('',(#5729,#5730,#5731,#5732));
#2442=EDGE_LOOP('',(#5733,#5734,#5735,#5736));
#2443=EDGE_LOOP('',(#5737,#5738,#5739,#5740));
#2444=EDGE_LOOP('',(#5741,#5742,#5743,#5744));
#2445=EDGE_LOOP('',(#5745,#5746,#5747,#5748));
#2446=EDGE_LOOP('',(#5749,#5750,#5751,#5752));
#2447=EDGE_LOOP('',(#5753,#5754,#5755,#5756));
#2448=EDGE_LOOP('',(#5757,#5758,#5759,#5760));
#2449=EDGE_LOOP('',(#5761,#5762,#5763,#5764));
#2450=EDGE_LOOP('',(#5765,#5766,#5767,#5768));
#2451=EDGE_LOOP('',(#5769,#5770,#5771,#5772));
#2452=EDGE_LOOP('',(#5773,#5774,#5775,#5776));
#2453=EDGE_LOOP('',(#5777,#5778,#5779,#5780));
#2454=EDGE_LOOP('',(#5781,#5782,#5783,#5784));
#2455=EDGE_LOOP('',(#5785,#5786,#5787,#5788));
#2456=EDGE_LOOP('',(#5789,#5790,#5791,#5792,#5793,#5794,#5795,#5796));
#2457=EDGE_LOOP('',(#5797,#5798,#5799,#5800,#5801,#5802,#5803,#5804,#5805,
#5806,#5807,#5808,#5809,#5810,#5811,#5812,#5813,#5814,#5815,#5816,#5817,
#5818,#5819,#5820,#5821,#5822,#5823,#5824,#5825,#5826));
#2458=EDGE_LOOP('',(#5827,#5828,#5829,#5830));
#2459=EDGE_LOOP('',(#5831,#5832,#5833,#5834,#5835,#5836,#5837,#5838,#5839,
#5840,#5841,#5842,#5843,#5844,#5845,#5846,#5847,#5848,#5849,#5850,#5851,
#5852,#5853,#5854,#5855,#5856,#5857,#5858,#5859,#5860,#5861));
#2460=EDGE_LOOP('',(#5862,#5863,#5864,#5865));
#2461=EDGE_LOOP('',(#5866,#5867,#5868,#5869));
#2462=EDGE_LOOP('',(#5870,#5871,#5872,#5873));
#2463=EDGE_LOOP('',(#5874,#5875,#5876,#5877));
#2464=EDGE_LOOP('',(#5878,#5879,#5880,#5881));
#2465=EDGE_LOOP('',(#5882,#5883,#5884,#5885));
#2466=EDGE_LOOP('',(#5886,#5887,#5888,#5889));
#2467=EDGE_LOOP('',(#5890,#5891,#5892,#5893,#5894,#5895));
#2468=EDGE_LOOP('',(#5896));
#2469=EDGE_LOOP('',(#5897,#5898,#5899,#5900));
#2470=EDGE_LOOP('',(#5901,#5902,#5903,#5904));
#2471=EDGE_LOOP('',(#5905));
#2472=EDGE_LOOP('',(#5906,#5907,#5908,#5909,#5910,#5911));
#2473=EDGE_LOOP('',(#5912));
#2474=CIRCLE('',#6656,3.5);
#2475=CIRCLE('',#6657,2.5);
#2476=CIRCLE('',#6659,3.5);
#2477=CIRCLE('',#6661,2.5);
#2478=CIRCLE('',#6663,3.5);
#2479=CIRCLE('',#6664,2.5);
#2480=CIRCLE('',#6666,3.5);
#2481=CIRCLE('',#6668,2.5);
#2482=CIRCLE('',#6670,3.5);
#2483=CIRCLE('',#6671,3.5);
#2484=CIRCLE('',#6673,3.5);
#2485=CIRCLE('',#6674,3.5);
#2486=CIRCLE('',#6676,3.5);
#2487=CIRCLE('',#6677,3.5);
#2488=CIRCLE('',#6679,3.5);
#2489=CIRCLE('',#6680,3.5);
#2490=CIRCLE('',#6705,1.666);
#2491=CIRCLE('',#6706,1.666);
#2492=CIRCLE('',#6721,1.666);
#2493=CIRCLE('',#6723,2.05475);
#2494=CIRCLE('',#6739,2.05475);
#2495=CIRCLE('',#6741,1.666);
#2496=CIRCLE('',#6742,1.666);
#2497=CIRCLE('',#6757,1.666);
#2498=CIRCLE('',#6759,2.05475);
#2499=CIRCLE('',#6775,2.05475);
#2500=CIRCLE('',#6785,2.);
#2501=CIRCLE('',#6786,2.);
#2502=CIRCLE('',#6788,4.);
#2503=CIRCLE('',#6789,4.);
#2504=CIRCLE('',#6791,4.);
#2505=CIRCLE('',#6792,4.);
#2506=CIRCLE('',#6829,2.5175);
#2507=CIRCLE('',#6839,2.5175);
#2508=CIRCLE('',#6841,3.0735);
#2509=CIRCLE('',#6851,3.0735);
#2510=CIRCLE('',#6853,26.9999999999999);
#2511=CIRCLE('',#6854,26.9999999999999);
#2512=CIRCLE('',#6856,2.);
#2513=CIRCLE('',#6857,2.);
#2514=CIRCLE('',#6859,23.0000000000001);
#2515=CIRCLE('',#6860,23.0000000000001);
#2516=CIRCLE('',#6862,2.);
#2517=CIRCLE('',#6863,2.);
#2518=CIRCLE('',#6866,6.);
#2519=CIRCLE('',#6869,3.);
#2520=CIRCLE('',#6870,3.);
#2521=CIRCLE('',#6872,3.);
#2522=CIRCLE('',#6873,3.);
#2523=CIRCLE('',#6875,5.);
#2524=CIRCLE('',#6876,5.);
#2525=CIRCLE('',#6878,6.);
#2526=CIRCLE('',#6880,10.);
#2527=CIRCLE('',#6881,10.);
#2528=CIRCLE('',#6883,6.);
#2529=CIRCLE('',#6884,8.);
#2530=CIRCLE('',#6885,6.);
#2531=CIRCLE('',#6890,6.);
#2532=CIRCLE('',#6891,8.);
#2533=CIRCLE('',#6892,6.);
#2534=CIRCLE('',#6902,3.);
#2535=CIRCLE('',#6903,3.);
#2536=CIRCLE('',#6906,3.);
#2537=CIRCLE('',#6907,3.);
#2538=CIRCLE('',#6928,2.);
#2539=CIRCLE('',#6929,2.);
#2540=CIRCLE('',#6931,3.);
#2541=CIRCLE('',#6933,3.);
#2542=CIRCLE('',#6935,3.);
#2543=CIRCLE('',#6937,5.);
#2544=CIRCLE('',#6938,3.);
#2545=CIRCLE('',#6940,5.);
#2546=CIRCLE('',#6946,3.);
#2547=CIRCLE('',#6947,3.);
#2548=CIRCLE('',#6949,4.);
#2549=CIRCLE('',#6951,4.);
#2550=CIRCLE('',#6953,4.);
#2551=CIRCLE('',#6955,7.);
#2552=CIRCLE('',#6956,4.);
#2553=CIRCLE('',#6958,7.);
#2554=CIRCLE('',#6964,3.);
#2555=CIRCLE('',#6965,3.);
#2556=CIRCLE('',#6967,5.);
#2557=CIRCLE('',#6968,5.);
#2558=CIRCLE('',#6975,5.);
#2559=CIRCLE('',#6976,2.);
#2560=CIRCLE('',#6978,2.);
#2561=CIRCLE('',#6980,5.);
#2562=CIRCLE('',#6984,4.);
#2563=CIRCLE('',#6985,4.);
#2564=CIRCLE('',#6987,5.);
#2565=CIRCLE('',#6988,5.);
#2566=CIRCLE('',#6993,4.);
#2567=CIRCLE('',#6994,4.);
#2568=CIRCLE('',#6996,7.);
#2569=CIRCLE('',#6997,7.);
#2570=CIRCLE('',#7002,4.);
#2571=CIRCLE('',#7003,4.);
#2572=CIRCLE('',#7005,8.);
#2573=CIRCLE('',#7006,8.);
#2574=CIRCLE('',#7013,7.);
#2575=CIRCLE('',#7014,3.);
#2576=CIRCLE('',#7016,3.);
#2577=CIRCLE('',#7018,7.);
#2578=CIRCLE('',#7022,1.5);
#2579=CIRCLE('',#7023,1.5);
#2580=CIRCLE('',#7025,2.);
#2581=CIRCLE('',#7027,2.);
#2582=CIRCLE('',#7029,2.);
#2583=CIRCLE('',#7031,4.);
#2584=CIRCLE('',#7032,2.);
#2585=CIRCLE('',#7034,4.);
#2586=CIRCLE('',#7040,2.);
#2587=CIRCLE('',#7041,2.);
#2588=CIRCLE('',#7043,4.);
#2589=CIRCLE('',#7044,4.);
#2590=CIRCLE('',#7049,2.);
#2591=CIRCLE('',#7050,2.);
#2592=CIRCLE('',#7052,4.);
#2593=CIRCLE('',#7053,4.);
#2594=CIRCLE('',#7060,3.5);
#2595=CIRCLE('',#7061,1.5);
#2596=CIRCLE('',#7063,1.5);
#2597=CIRCLE('',#7065,3.5);
#2598=CIRCLE('',#7069,4.);
#2599=CIRCLE('',#7070,4.);
#2600=CIRCLE('',#7072,14.);
#2601=CIRCLE('',#7073,14.);
#2602=CIRCLE('',#7078,2.37175);
#2603=CIRCLE('',#7087,2.942);
#2604=CIRCLE('',#7095,2.);
#2605=CIRCLE('',#7096,2.37175);
#2606=CIRCLE('',#7098,2.942);
#2607=CIRCLE('',#7108,6.);
#2608=CIRCLE('',#7109,4.);
#2609=CIRCLE('',#7111,6.);
#2610=CIRCLE('',#7114,4.);
#2611=CIRCLE('',#7119,1.954);
#2612=CIRCLE('',#7133,1.5555);
#2613=CIRCLE('',#7147,1.954);
#2614=CIRCLE('',#7148,1.);
#2615=CIRCLE('',#7150,1.5555);
#2616=CIRCLE('',#7160,3.5);
#2617=CIRCLE('',#7162,3.5);
#2618=VERTEX_POINT('',#8735);
#2619=VERTEX_POINT('',#8737);
#2620=VERTEX_POINT('',#8740);
#2621=VERTEX_POINT('',#8744);
#2622=VERTEX_POINT('',#8748);
#2623=VERTEX_POINT('',#8750);
#2624=VERTEX_POINT('',#8753);
#2625=VERTEX_POINT('',#8757);
#2626=VERTEX_POINT('',#8761);
#2627=VERTEX_POINT('',#8763);
#2628=VERTEX_POINT('',#8767);
#2629=VERTEX_POINT('',#8769);
#2630=VERTEX_POINT('',#8773);
#2631=VERTEX_POINT('',#8775);
#2632=VERTEX_POINT('',#8779);
#2633=VERTEX_POINT('',#8781);
#2634=VERTEX_POINT('',#8785);
#2635=VERTEX_POINT('',#8786);
#2636=VERTEX_POINT('',#8788);
#2637=VERTEX_POINT('',#8790);
#2638=VERTEX_POINT('',#8794);
#2639=VERTEX_POINT('',#8796);
#2640=VERTEX_POINT('',#8800);
#2641=VERTEX_POINT('',#8802);
#2642=VERTEX_POINT('',#8809);
#2643=VERTEX_POINT('',#8810);
#2644=VERTEX_POINT('',#8812);
#2645=VERTEX_POINT('',#8814);
#2646=VERTEX_POINT('',#8818);
#2647=VERTEX_POINT('',#8820);
#2648=VERTEX_POINT('',#8824);
#2649=VERTEX_POINT('',#8826);
#2650=VERTEX_POINT('',#8833);
#2651=VERTEX_POINT('',#8834);
#2652=VERTEX_POINT('',#8836);
#2653=VERTEX_POINT('',#8838);
#2654=VERTEX_POINT('',#8842);
#2655=VERTEX_POINT('',#8843);
#2656=VERTEX_POINT('',#8845);
#2657=VERTEX_POINT('',#8847);
#2658=VERTEX_POINT('',#8854);
#2659=VERTEX_POINT('',#8856);
#2660=VERTEX_POINT('',#8860);
#2661=VERTEX_POINT('',#8862);
#2662=VERTEX_POINT('',#8866);
#2663=VERTEX_POINT('',#8868);
#2664=VERTEX_POINT('',#8872);
#2665=VERTEX_POINT('',#8873);
#2666=VERTEX_POINT('',#8875);
#2667=VERTEX_POINT('',#8877);
#2668=VERTEX_POINT('',#8884);
#2669=VERTEX_POINT('',#8886);
#2670=VERTEX_POINT('',#8890);
#2671=VERTEX_POINT('',#8891);
#2672=VERTEX_POINT('',#8896);
#2673=VERTEX_POINT('',#8900);
#2674=VERTEX_POINT('',#8908);
#2675=VERTEX_POINT('',#8909);
#2676=VERTEX_POINT('',#8911);
#2677=VERTEX_POINT('',#8931);
#2678=VERTEX_POINT('',#8933);
#2679=VERTEX_POINT('',#8938);
#2680=VERTEX_POINT('',#8964);
#2681=VERTEX_POINT('',#8965);
#2682=VERTEX_POINT('',#9015);
#2683=VERTEX_POINT('',#9016);
#2684=VERTEX_POINT('',#9063);
#2685=VERTEX_POINT('',#9064);
#2686=VERTEX_POINT('',#9114);
#2687=VERTEX_POINT('',#9115);
#2688=VERTEX_POINT('',#9165);
#2689=VERTEX_POINT('',#9166);
#2690=VERTEX_POINT('',#9213);
#2691=VERTEX_POINT('',#9214);
#2692=VERTEX_POINT('',#9261);
#2693=VERTEX_POINT('',#9262);
#2694=VERTEX_POINT('',#9312);
#2695=VERTEX_POINT('',#9313);
#2696=VERTEX_POINT('',#9360);
#2697=VERTEX_POINT('',#9361);
#2698=VERTEX_POINT('',#9408);
#2699=VERTEX_POINT('',#9409);
#2700=VERTEX_POINT('',#9459);
#2701=VERTEX_POINT('',#9460);
#2702=VERTEX_POINT('',#9510);
#2703=VERTEX_POINT('',#9511);
#2704=VERTEX_POINT('',#9558);
#2705=VERTEX_POINT('',#9559);
#2706=VERTEX_POINT('',#9609);
#2707=VERTEX_POINT('',#9610);
#2708=VERTEX_POINT('',#9612);
#2709=VERTEX_POINT('',#9626);
#2710=VERTEX_POINT('',#9648);
#2711=VERTEX_POINT('',#9649);
#2712=VERTEX_POINT('',#9651);
#2713=VERTEX_POINT('',#9658);
#2714=VERTEX_POINT('',#9668);
#2715=VERTEX_POINT('',#9669);
#2716=VERTEX_POINT('',#9692);
#2717=VERTEX_POINT('',#9693);
#2718=VERTEX_POINT('',#9717);
#2719=VERTEX_POINT('',#9718);
#2720=VERTEX_POINT('',#9742);
#2721=VERTEX_POINT('',#9743);
#2722=VERTEX_POINT('',#9766);
#2723=VERTEX_POINT('',#9767);
#2724=VERTEX_POINT('',#9791);
#2725=VERTEX_POINT('',#9792);
#2726=VERTEX_POINT('',#9815);
#2727=VERTEX_POINT('',#9816);
#2728=VERTEX_POINT('',#9840);
#2729=VERTEX_POINT('',#9841);
#2730=VERTEX_POINT('',#9865);
#2731=VERTEX_POINT('',#9866);
#2732=VERTEX_POINT('',#9889);
#2733=VERTEX_POINT('',#9890);
#2734=VERTEX_POINT('',#9914);
#2735=VERTEX_POINT('',#9915);
#2736=VERTEX_POINT('',#9938);
#2737=VERTEX_POINT('',#9939);
#2738=VERTEX_POINT('',#9963);
#2739=VERTEX_POINT('',#9964);
#2740=VERTEX_POINT('',#9988);
#2741=VERTEX_POINT('',#9989);
#2742=VERTEX_POINT('',#10012);
#2743=VERTEX_POINT('',#10013);
#2744=VERTEX_POINT('',#10015);
#2745=VERTEX_POINT('',#10021);
#2746=VERTEX_POINT('',#10029);
#2747=VERTEX_POINT('',#10030);
#2748=VERTEX_POINT('',#10032);
#2749=VERTEX_POINT('',#10052);
#2750=VERTEX_POINT('',#10054);
#2751=VERTEX_POINT('',#10059);
#2752=VERTEX_POINT('',#10085);
#2753=VERTEX_POINT('',#10086);
#2754=VERTEX_POINT('',#10136);
#2755=VERTEX_POINT('',#10137);
#2756=VERTEX_POINT('',#10184);
#2757=VERTEX_POINT('',#10185);
#2758=VERTEX_POINT('',#10235);
#2759=VERTEX_POINT('',#10236);
#2760=VERTEX_POINT('',#10286);
#2761=VERTEX_POINT('',#10287);
#2762=VERTEX_POINT('',#10334);
#2763=VERTEX_POINT('',#10335);
#2764=VERTEX_POINT('',#10382);
#2765=VERTEX_POINT('',#10383);
#2766=VERTEX_POINT('',#10433);
#2767=VERTEX_POINT('',#10434);
#2768=VERTEX_POINT('',#10481);
#2769=VERTEX_POINT('',#10482);
#2770=VERTEX_POINT('',#10529);
#2771=VERTEX_POINT('',#10530);
#2772=VERTEX_POINT('',#10580);
#2773=VERTEX_POINT('',#10581);
#2774=VERTEX_POINT('',#10631);
#2775=VERTEX_POINT('',#10632);
#2776=VERTEX_POINT('',#10679);
#2777=VERTEX_POINT('',#10680);
#2778=VERTEX_POINT('',#10730);
#2779=VERTEX_POINT('',#10731);
#2780=VERTEX_POINT('',#10733);
#2781=VERTEX_POINT('',#10747);
#2782=VERTEX_POINT('',#10769);
#2783=VERTEX_POINT('',#10770);
#2784=VERTEX_POINT('',#10772);
#2785=VERTEX_POINT('',#10779);
#2786=VERTEX_POINT('',#10789);
#2787=VERTEX_POINT('',#10790);
#2788=VERTEX_POINT('',#10813);
#2789=VERTEX_POINT('',#10814);
#2790=VERTEX_POINT('',#10838);
#2791=VERTEX_POINT('',#10839);
#2792=VERTEX_POINT('',#10863);
#2793=VERTEX_POINT('',#10864);
#2794=VERTEX_POINT('',#10887);
#2795=VERTEX_POINT('',#10888);
#2796=VERTEX_POINT('',#10912);
#2797=VERTEX_POINT('',#10913);
#2798=VERTEX_POINT('',#10936);
#2799=VERTEX_POINT('',#10937);
#2800=VERTEX_POINT('',#10961);
#2801=VERTEX_POINT('',#10962);
#2802=VERTEX_POINT('',#10986);
#2803=VERTEX_POINT('',#10987);
#2804=VERTEX_POINT('',#11010);
#2805=VERTEX_POINT('',#11011);
#2806=VERTEX_POINT('',#11035);
#2807=VERTEX_POINT('',#11036);
#2808=VERTEX_POINT('',#11059);
#2809=VERTEX_POINT('',#11060);
#2810=VERTEX_POINT('',#11084);
#2811=VERTEX_POINT('',#11085);
#2812=VERTEX_POINT('',#11109);
#2813=VERTEX_POINT('',#11110);
#2814=VERTEX_POINT('',#11133);
#2815=VERTEX_POINT('',#11134);
#2816=VERTEX_POINT('',#11136);
#2817=VERTEX_POINT('',#11142);
#2818=VERTEX_POINT('',#13638);
#2819=VERTEX_POINT('',#13640);
#2820=VERTEX_POINT('',#13644);
#2821=VERTEX_POINT('',#13646);
#2822=VERTEX_POINT('',#13650);
#2823=VERTEX_POINT('',#13652);
#2824=VERTEX_POINT('',#13656);
#2825=VERTEX_POINT('',#13657);
#2826=VERTEX_POINT('',#13659);
#2827=VERTEX_POINT('',#13661);
#2828=VERTEX_POINT('',#13665);
#2829=VERTEX_POINT('',#13666);
#2830=VERTEX_POINT('',#13668);
#2831=VERTEX_POINT('',#13670);
#2832=VERTEX_POINT('',#13677);
#2833=VERTEX_POINT('',#13679);
#2834=VERTEX_POINT('',#13683);
#2835=VERTEX_POINT('',#13685);
#2836=VERTEX_POINT('',#13689);
#2837=VERTEX_POINT('',#13690);
#2838=VERTEX_POINT('',#13692);
#2839=VERTEX_POINT('',#13694);
#2840=VERTEX_POINT('',#13698);
#2841=VERTEX_POINT('',#13700);
#2842=VERTEX_POINT('',#13704);
#2843=VERTEX_POINT('',#13706);
#2844=VERTEX_POINT('',#13712);
#2845=VERTEX_POINT('',#13714);
#2846=VERTEX_POINT('',#13716);
#2847=VERTEX_POINT('',#13718);
#2848=VERTEX_POINT('',#13720);
#2849=VERTEX_POINT('',#13722);
#2850=VERTEX_POINT('',#13724);
#2851=VERTEX_POINT('',#13726);
#2852=VERTEX_POINT('',#13729);
#2853=VERTEX_POINT('',#13730);
#2854=VERTEX_POINT('',#13732);
#2855=VERTEX_POINT('',#13734);
#2856=VERTEX_POINT('',#13737);
#2857=VERTEX_POINT('',#13738);
#2858=VERTEX_POINT('',#13740);
#2859=VERTEX_POINT('',#13742);
#2860=VERTEX_POINT('',#13753);
#2861=VERTEX_POINT('',#13755);
#2862=VERTEX_POINT('',#13757);
#2863=VERTEX_POINT('',#13759);
#2864=VERTEX_POINT('',#13761);
#2865=VERTEX_POINT('',#13763);
#2866=VERTEX_POINT('',#13767);
#2867=VERTEX_POINT('',#13768);
#2868=VERTEX_POINT('',#13773);
#2869=VERTEX_POINT('',#13777);
#2870=VERTEX_POINT('',#13783);
#2871=VERTEX_POINT('',#13784);
#2872=VERTEX_POINT('',#13789);
#2873=VERTEX_POINT('',#13793);
#2874=VERTEX_POINT('',#13799);
#2875=VERTEX_POINT('',#13800);
#2876=VERTEX_POINT('',#13803);
#2877=VERTEX_POINT('',#13805);
#2878=VERTEX_POINT('',#13807);
#2879=VERTEX_POINT('',#13809);
#2880=VERTEX_POINT('',#13813);
#2881=VERTEX_POINT('',#13817);
#2882=VERTEX_POINT('',#13819);
#2883=VERTEX_POINT('',#13823);
#2884=VERTEX_POINT('',#13827);
#2885=VERTEX_POINT('',#13829);
#2886=VERTEX_POINT('',#13837);
#2887=VERTEX_POINT('',#13841);
#2888=VERTEX_POINT('',#13851);
#2889=VERTEX_POINT('',#13852);
#2890=VERTEX_POINT('',#13854);
#2891=VERTEX_POINT('',#13859);
#2892=VERTEX_POINT('',#13872);
#2893=VERTEX_POINT('',#13873);
#2894=VERTEX_POINT('',#13923);
#2895=VERTEX_POINT('',#13924);
#2896=VERTEX_POINT('',#13974);
#2897=VERTEX_POINT('',#13975);
#2898=VERTEX_POINT('',#14022);
#2899=VERTEX_POINT('',#14023);
#2900=VERTEX_POINT('',#14070);
#2901=VERTEX_POINT('',#14071);
#2902=VERTEX_POINT('',#14121);
#2903=VERTEX_POINT('',#14122);
#2904=VERTEX_POINT('',#14172);
#2905=VERTEX_POINT('',#14173);
#2906=VERTEX_POINT('',#14220);
#2907=VERTEX_POINT('',#14221);
#2908=VERTEX_POINT('',#14271);
#2909=VERTEX_POINT('',#14272);
#2910=VERTEX_POINT('',#14274);
#2911=VERTEX_POINT('',#14288);
#2912=VERTEX_POINT('',#14310);
#2913=VERTEX_POINT('',#14311);
#2914=VERTEX_POINT('',#14313);
#2915=VERTEX_POINT('',#14322);
#2916=VERTEX_POINT('',#14334);
#2917=VERTEX_POINT('',#14335);
#2918=VERTEX_POINT('',#14358);
#2919=VERTEX_POINT('',#14359);
#2920=VERTEX_POINT('',#14383);
#2921=VERTEX_POINT('',#14384);
#2922=VERTEX_POINT('',#14407);
#2923=VERTEX_POINT('',#14408);
#2924=VERTEX_POINT('',#14432);
#2925=VERTEX_POINT('',#14433);
#2926=VERTEX_POINT('',#14456);
#2927=VERTEX_POINT('',#14457);
#2928=VERTEX_POINT('',#14481);
#2929=VERTEX_POINT('',#14482);
#2930=VERTEX_POINT('',#14506);
#2931=VERTEX_POINT('',#14507);
#2932=VERTEX_POINT('',#14530);
#2933=VERTEX_POINT('',#14531);
#2934=VERTEX_POINT('',#14533);
#2935=VERTEX_POINT('',#14539);
#2936=VERTEX_POINT('',#14547);
#2937=VERTEX_POINT('',#14548);
#2938=VERTEX_POINT('',#14550);
#2939=VERTEX_POINT('',#14552);
#2940=VERTEX_POINT('',#14556);
#2941=VERTEX_POINT('',#14558);
#2942=VERTEX_POINT('',#14562);
#2943=VERTEX_POINT('',#14564);
#2944=VERTEX_POINT('',#15566);
#2945=VERTEX_POINT('',#15570);
#2946=VERTEX_POINT('',#15572);
#2947=VERTEX_POINT('',#15576);
#2948=VERTEX_POINT('',#15578);
#2949=VERTEX_POINT('',#15582);
#2950=VERTEX_POINT('',#15584);
#2951=VERTEX_POINT('',#15588);
#2952=VERTEX_POINT('',#15592);
#2953=VERTEX_POINT('',#15593);
#2954=VERTEX_POINT('',#15595);
#2955=VERTEX_POINT('',#15597);
#2956=VERTEX_POINT('',#15601);
#2957=VERTEX_POINT('',#15603);
#2958=VERTEX_POINT('',#15605);
#2959=VERTEX_POINT('',#15607);
#2960=VERTEX_POINT('',#15609);
#2961=VERTEX_POINT('',#15611);
#2962=VERTEX_POINT('',#15613);
#2963=VERTEX_POINT('',#15615);
#2964=VERTEX_POINT('',#15619);
#2965=VERTEX_POINT('',#15623);
#2966=VERTEX_POINT('',#15627);
#2967=VERTEX_POINT('',#15631);
#2968=VERTEX_POINT('',#15633);
#2969=VERTEX_POINT('',#15635);
#2970=VERTEX_POINT('',#15637);
#2971=VERTEX_POINT('',#15639);
#2972=VERTEX_POINT('',#15655);
#2973=VERTEX_POINT('',#15656);
#2974=VERTEX_POINT('',#15658);
#2975=VERTEX_POINT('',#15660);
#2976=VERTEX_POINT('',#15664);
#2977=VERTEX_POINT('',#15666);
#2978=VERTEX_POINT('',#15670);
#2979=VERTEX_POINT('',#15672);
#2980=VERTEX_POINT('',#15679);
#2981=VERTEX_POINT('',#15680);
#2982=VERTEX_POINT('',#15682);
#2983=VERTEX_POINT('',#15684);
#2984=VERTEX_POINT('',#15688);
#2985=VERTEX_POINT('',#15689);
#2986=VERTEX_POINT('',#15691);
#2987=VERTEX_POINT('',#15693);
#2988=VERTEX_POINT('',#15697);
#2989=VERTEX_POINT('',#15699);
#2990=VERTEX_POINT('',#15704);
#2991=VERTEX_POINT('',#15708);
#2992=VERTEX_POINT('',#15716);
#2993=VERTEX_POINT('',#15718);
#2994=VERTEX_POINT('',#15722);
#2995=VERTEX_POINT('',#15724);
#2996=VERTEX_POINT('',#15728);
#2997=VERTEX_POINT('',#15729);
#2998=VERTEX_POINT('',#15734);
#2999=VERTEX_POINT('',#15735);
#3000=VERTEX_POINT('',#15740);
#3001=VERTEX_POINT('',#15742);
#3002=VERTEX_POINT('',#15746);
#3003=VERTEX_POINT('',#15747);
#3004=VERTEX_POINT('',#15750);
#3005=VERTEX_POINT('',#15754);
#3006=VERTEX_POINT('',#15756);
#3007=VERTEX_POINT('',#15760);
#3008=VERTEX_POINT('',#15770);
#3009=VERTEX_POINT('',#15772);
#3010=VERTEX_POINT('',#15776);
#3011=VERTEX_POINT('',#15779);
#3012=VERTEX_POINT('',#15782);
#3013=VERTEX_POINT('',#15786);
#3014=VERTEX_POINT('',#15788);
#3015=VERTEX_POINT('',#15791);
#3016=VERTEX_POINT('',#15800);
#3017=VERTEX_POINT('',#15802);
#3018=VERTEX_POINT('',#15806);
#3019=VERTEX_POINT('',#15809);
#3020=VERTEX_POINT('',#15812);
#3021=VERTEX_POINT('',#15816);
#3022=VERTEX_POINT('',#15818);
#3023=VERTEX_POINT('',#15821);
#3024=VERTEX_POINT('',#15830);
#3025=VERTEX_POINT('',#15832);
#3026=VERTEX_POINT('',#15836);
#3027=VERTEX_POINT('',#15838);
#3028=VERTEX_POINT('',#15845);
#3029=VERTEX_POINT('',#15846);
#3030=VERTEX_POINT('',#15848);
#3031=VERTEX_POINT('',#15850);
#3032=VERTEX_POINT('',#15854);
#3033=VERTEX_POINT('',#15855);
#3034=VERTEX_POINT('',#15857);
#3035=VERTEX_POINT('',#15859);
#3036=VERTEX_POINT('',#15872);
#3037=VERTEX_POINT('',#15874);
#3038=VERTEX_POINT('',#15878);
#3039=VERTEX_POINT('',#15880);
#3040=VERTEX_POINT('',#15887);
#3041=VERTEX_POINT('',#15889);
#3042=VERTEX_POINT('',#15893);
#3043=VERTEX_POINT('',#15895);
#3044=VERTEX_POINT('',#15902);
#3045=VERTEX_POINT('',#15904);
#3046=VERTEX_POINT('',#15908);
#3047=VERTEX_POINT('',#15910);
#3048=VERTEX_POINT('',#15917);
#3049=VERTEX_POINT('',#15918);
#3050=VERTEX_POINT('',#15920);
#3051=VERTEX_POINT('',#15922);
#3052=VERTEX_POINT('',#15926);
#3053=VERTEX_POINT('',#15927);
#3054=VERTEX_POINT('',#15929);
#3055=VERTEX_POINT('',#15931);
#3056=VERTEX_POINT('',#15944);
#3057=VERTEX_POINT('',#15946);
#3058=VERTEX_POINT('',#15950);
#3059=VERTEX_POINT('',#15953);
#3060=VERTEX_POINT('',#15956);
#3061=VERTEX_POINT('',#15960);
#3062=VERTEX_POINT('',#15962);
#3063=VERTEX_POINT('',#15965);
#3064=VERTEX_POINT('',#15974);
#3065=VERTEX_POINT('',#15976);
#3066=VERTEX_POINT('',#15980);
#3067=VERTEX_POINT('',#15982);
#3068=VERTEX_POINT('',#15989);
#3069=VERTEX_POINT('',#15991);
#3070=VERTEX_POINT('',#15995);
#3071=VERTEX_POINT('',#15997);
#3072=VERTEX_POINT('',#16004);
#3073=VERTEX_POINT('',#16005);
#3074=VERTEX_POINT('',#16007);
#3075=VERTEX_POINT('',#16009);
#3076=VERTEX_POINT('',#16013);
#3077=VERTEX_POINT('',#16014);
#3078=VERTEX_POINT('',#16016);
#3079=VERTEX_POINT('',#16018);
#3080=VERTEX_POINT('',#16031);
#3081=VERTEX_POINT('',#16033);
#3082=VERTEX_POINT('',#16037);
#3083=VERTEX_POINT('',#16039);
#3084=VERTEX_POINT('',#16046);
#3085=VERTEX_POINT('',#16047);
#3086=VERTEX_POINT('',#16049);
#3087=VERTEX_POINT('',#16056);
#3088=VERTEX_POINT('',#16063);
#3089=VERTEX_POINT('',#16064);
#3090=VERTEX_POINT('',#16088);
#3091=VERTEX_POINT('',#16089);
#3092=VERTEX_POINT('',#16112);
#3093=VERTEX_POINT('',#16113);
#3094=VERTEX_POINT('',#16137);
#3095=VERTEX_POINT('',#16138);
#3096=VERTEX_POINT('',#16162);
#3097=VERTEX_POINT('',#16163);
#3098=VERTEX_POINT('',#16186);
#3099=VERTEX_POINT('',#16187);
#3100=VERTEX_POINT('',#16210);
#3101=VERTEX_POINT('',#16211);
#3102=VERTEX_POINT('',#16235);
#3103=VERTEX_POINT('',#16236);
#3104=VERTEX_POINT('',#16238);
#3105=VERTEX_POINT('',#16252);
#3106=VERTEX_POINT('',#16262);
#3107=VERTEX_POINT('',#16263);
#3108=VERTEX_POINT('',#16310);
#3109=VERTEX_POINT('',#16311);
#3110=VERTEX_POINT('',#16358);
#3111=VERTEX_POINT('',#16359);
#3112=VERTEX_POINT('',#16406);
#3113=VERTEX_POINT('',#16407);
#3114=VERTEX_POINT('',#16460);
#3115=VERTEX_POINT('',#16461);
#3116=VERTEX_POINT('',#16508);
#3117=VERTEX_POINT('',#16509);
#3118=VERTEX_POINT('',#16556);
#3119=VERTEX_POINT('',#16558);
#3120=VERTEX_POINT('',#16560);
#3121=VERTEX_POINT('',#16640);
#3122=VERTEX_POINT('',#17093);
#3123=VERTEX_POINT('',#17207);
#3124=VERTEX_POINT('',#17229);
#3125=VERTEX_POINT('',#17230);
#3126=VERTEX_POINT('',#17232);
#3127=VERTEX_POINT('',#17234);
#3128=VERTEX_POINT('',#17238);
#3129=VERTEX_POINT('',#17240);
#3130=VERTEX_POINT('',#17244);
#3131=VERTEX_POINT('',#17246);
#3132=VERTEX_POINT('',#17250);
#3133=VERTEX_POINT('',#17252);
#3134=VERTEX_POINT('',#17256);
#3135=VERTEX_POINT('',#17258);
#3136=VERTEX_POINT('',#17572);
#3137=VERTEX_POINT('',#17574);
#3138=VERTEX_POINT('',#17577);
#3139=VERTEX_POINT('',#17582);
#3140=VERTEX_POINT('',#17589);
#3141=VERTEX_POINT('',#17590);
#3142=VERTEX_POINT('',#17592);
#3143=VERTEX_POINT('',#17603);
#3144=VERTEX_POINT('',#17613);
#3145=VERTEX_POINT('',#17614);
#3146=VERTEX_POINT('',#17661);
#3147=VERTEX_POINT('',#17662);
#3148=VERTEX_POINT('',#17709);
#3149=VERTEX_POINT('',#17710);
#3150=VERTEX_POINT('',#17760);
#3151=VERTEX_POINT('',#17761);
#3152=VERTEX_POINT('',#17808);
#3153=VERTEX_POINT('',#17809);
#3154=VERTEX_POINT('',#17856);
#3155=VERTEX_POINT('',#17857);
#3156=VERTEX_POINT('',#17904);
#3157=VERTEX_POINT('',#17905);
#3158=VERTEX_POINT('',#17958);
#3159=VERTEX_POINT('',#17959);
#3160=VERTEX_POINT('',#18006);
#3161=VERTEX_POINT('',#18007);
#3162=VERTEX_POINT('',#18054);
#3163=VERTEX_POINT('',#18055);
#3164=VERTEX_POINT('',#18108);
#3165=VERTEX_POINT('',#18109);
#3166=VERTEX_POINT('',#18156);
#3167=VERTEX_POINT('',#18157);
#3168=VERTEX_POINT('',#18204);
#3169=VERTEX_POINT('',#18205);
#3170=VERTEX_POINT('',#18207);
#3171=VERTEX_POINT('',#18217);
#3172=VERTEX_POINT('',#18228);
#3173=VERTEX_POINT('',#18229);
#3174=VERTEX_POINT('',#18252);
#3175=VERTEX_POINT('',#18253);
#3176=VERTEX_POINT('',#18276);
#3177=VERTEX_POINT('',#18277);
#3178=VERTEX_POINT('',#18301);
#3179=VERTEX_POINT('',#18302);
#3180=VERTEX_POINT('',#18326);
#3181=VERTEX_POINT('',#18327);
#3182=VERTEX_POINT('',#18350);
#3183=VERTEX_POINT('',#18351);
#3184=VERTEX_POINT('',#18375);
#3185=VERTEX_POINT('',#18376);
#3186=VERTEX_POINT('',#18400);
#3187=VERTEX_POINT('',#18401);
#3188=VERTEX_POINT('',#18424);
#3189=VERTEX_POINT('',#18425);
#3190=VERTEX_POINT('',#18448);
#3191=VERTEX_POINT('',#18449);
#3192=VERTEX_POINT('',#18473);
#3193=VERTEX_POINT('',#18474);
#3194=VERTEX_POINT('',#18498);
#3195=VERTEX_POINT('',#18499);
#3196=VERTEX_POINT('',#18522);
#3197=VERTEX_POINT('',#18686);
#3198=VERTEX_POINT('',#18745);
#3199=VERTEX_POINT('',#18811);
#3200=VERTEX_POINT('',#19166);
#3201=VERTEX_POINT('',#19277);
#3202=VERTEX_POINT('',#19751);
#3203=VERTEX_POINT('',#19752);
#3204=VERTEX_POINT('',#19754);
#3205=VERTEX_POINT('',#19756);
#3206=VERTEX_POINT('',#19760);
#3207=VERTEX_POINT('',#19762);
#3208=VERTEX_POINT('',#19766);
#3209=VERTEX_POINT('',#19768);
#3210=VERTEX_POINT('',#19772);
#3211=VERTEX_POINT('',#19774);
#3212=VERTEX_POINT('',#19778);
#3213=VERTEX_POINT('',#19780);
#3214=VERTEX_POINT('',#19788);
#3215=VERTEX_POINT('',#19791);
#3216=EDGE_CURVE('',#2618,#2618,#2474,.T.);
#3217=EDGE_CURVE('',#2619,#2619,#2475,.T.);
#3218=EDGE_CURVE('',#2620,#2620,#2476,.T.);
#3219=EDGE_CURVE('',#2620,#2618,#493,.T.);
#3220=EDGE_CURVE('',#2619,#2621,#494,.T.);
#3221=EDGE_CURVE('',#2621,#2621,#2477,.T.);
#3222=EDGE_CURVE('',#2622,#2622,#2478,.T.);
#3223=EDGE_CURVE('',#2623,#2623,#2479,.T.);
#3224=EDGE_CURVE('',#2624,#2624,#2480,.T.);
#3225=EDGE_CURVE('',#2624,#2622,#495,.T.);
#3226=EDGE_CURVE('',#2623,#2625,#496,.T.);
#3227=EDGE_CURVE('',#2625,#2625,#2481,.T.);
#3228=EDGE_CURVE('',#2626,#2626,#2482,.T.);
#3229=EDGE_CURVE('',#2626,#2627,#497,.T.);
#3230=EDGE_CURVE('',#2627,#2627,#2483,.T.);
#3231=EDGE_CURVE('',#2628,#2628,#2484,.T.);
#3232=EDGE_CURVE('',#2628,#2629,#498,.T.);
#3233=EDGE_CURVE('',#2629,#2629,#2485,.T.);
#3234=EDGE_CURVE('',#2630,#2630,#2486,.T.);
#3235=EDGE_CURVE('',#2630,#2631,#499,.T.);
#3236=EDGE_CURVE('',#2631,#2631,#2487,.T.);
#3237=EDGE_CURVE('',#2632,#2632,#2488,.T.);
#3238=EDGE_CURVE('',#2632,#2633,#500,.T.);
#3239=EDGE_CURVE('',#2633,#2633,#2489,.T.);
#3240=EDGE_CURVE('',#2634,#2635,#501,.T.);
#3241=EDGE_CURVE('',#2634,#2636,#502,.T.);
#3242=EDGE_CURVE('',#2637,#2636,#503,.T.);
#3243=EDGE_CURVE('',#2635,#2637,#504,.T.);
#3244=EDGE_CURVE('',#2638,#2634,#505,.T.);
#3245=EDGE_CURVE('',#2638,#2639,#506,.T.);
#3246=EDGE_CURVE('',#2636,#2639,#507,.T.);
#3247=EDGE_CURVE('',#2640,#2638,#508,.T.);
#3248=EDGE_CURVE('',#2640,#2641,#509,.T.);
#3249=EDGE_CURVE('',#2639,#2641,#510,.T.);
#3250=EDGE_CURVE('',#2635,#2640,#511,.T.);
#3251=EDGE_CURVE('',#2641,#2637,#512,.T.);
#3252=EDGE_CURVE('',#2642,#2643,#513,.T.);
#3253=EDGE_CURVE('',#2642,#2644,#514,.T.);
#3254=EDGE_CURVE('',#2645,#2644,#515,.T.);
#3255=EDGE_CURVE('',#2643,#2645,#516,.T.);
#3256=EDGE_CURVE('',#2646,#2642,#517,.T.);
#3257=EDGE_CURVE('',#2646,#2647,#518,.T.);
#3258=EDGE_CURVE('',#2644,#2647,#519,.T.);
#3259=EDGE_CURVE('',#2648,#2646,#520,.T.);
#3260=EDGE_CURVE('',#2648,#2649,#521,.T.);
#3261=EDGE_CURVE('',#2647,#2649,#522,.T.);
#3262=EDGE_CURVE('',#2643,#2648,#523,.T.);
#3263=EDGE_CURVE('',#2649,#2645,#524,.T.);
#3264=EDGE_CURVE('',#2650,#2651,#525,.T.);
#3265=EDGE_CURVE('',#2650,#2652,#526,.F.);
#3266=EDGE_CURVE('',#2653,#2652,#527,.T.);
#3267=EDGE_CURVE('',#2651,#2653,#528,.T.);
#3268=EDGE_CURVE('',#2654,#2655,#529,.T.);
#3269=EDGE_CURVE('',#2654,#2656,#530,.T.);
#3270=EDGE_CURVE('',#2657,#2656,#531,.T.);
#3271=EDGE_CURVE('',#2655,#2657,#532,.T.);
#3272=EDGE_CURVE('',#2652,#2657,#533,.F.);
#3273=EDGE_CURVE('',#2656,#2653,#534,.T.);
#3274=EDGE_CURVE('',#2651,#2658,#535,.T.);
#3275=EDGE_CURVE('',#2658,#2659,#536,.F.);
#3276=EDGE_CURVE('',#2659,#2650,#537,.F.);
#3277=EDGE_CURVE('',#2655,#2660,#538,.F.);
#3278=EDGE_CURVE('',#2660,#2661,#539,.T.);
#3279=EDGE_CURVE('',#2661,#2654,#540,.T.);
#3280=EDGE_CURVE('',#2660,#2662,#541,.F.);
#3281=EDGE_CURVE('',#2663,#2662,#542,.T.);
#3282=EDGE_CURVE('',#2661,#2663,#543,.T.);
#3283=EDGE_CURVE('',#2664,#2665,#544,.T.);
#3284=EDGE_CURVE('',#2664,#2666,#545,.T.);
#3285=EDGE_CURVE('',#2667,#2666,#546,.T.);
#3286=EDGE_CURVE('',#2665,#2667,#547,.T.);
#3287=EDGE_CURVE('',#2662,#2667,#548,.F.);
#3288=EDGE_CURVE('',#2666,#2663,#549,.T.);
#3289=EDGE_CURVE('',#2665,#2668,#550,.F.);
#3290=EDGE_CURVE('',#2668,#2669,#551,.F.);
#3291=EDGE_CURVE('',#2669,#2664,#552,.T.);
#3292=EDGE_CURVE('',#2670,#2671,#553,.F.);
#3293=EDGE_CURVE('',#2671,#2659,#554,.F.);
#3294=EDGE_CURVE('',#2670,#2658,#555,.F.);
#3295=EDGE_CURVE('',#2672,#2670,#556,.T.);
#3296=EDGE_CURVE('',#2672,#2669,#557,.T.);
#3297=EDGE_CURVE('',#2673,#2672,#558,.F.);
#3298=EDGE_CURVE('',#2673,#2668,#559,.T.);
#3299=EDGE_CURVE('',#2671,#2673,#560,.F.);
#3300=EDGE_CURVE('',#2674,#2675,#561,.T.);
#3301=EDGE_CURVE('',#2675,#2676,#127,.T.);
#3302=EDGE_CURVE('',#2676,#2677,#2490,.T.);
#3303=EDGE_CURVE('',#2677,#2678,#128,.T.);
#3304=EDGE_CURVE('',#2678,#2679,#562,.T.);
#3305=EDGE_CURVE('',#2679,#2679,#2491,.F.);
#3306=EDGE_CURVE('',#2678,#2674,#129,.T.);
#3307=EDGE_CURVE('',#2680,#2681,#563,.T.);
#3308=EDGE_CURVE('',#2681,#2675,#130,.T.);
#3309=EDGE_CURVE('',#2674,#2680,#131,.T.);
#3310=EDGE_CURVE('',#2682,#2683,#564,.T.);
#3311=EDGE_CURVE('',#2683,#2681,#132,.T.);
#3312=EDGE_CURVE('',#2680,#2682,#133,.T.);
#3313=EDGE_CURVE('',#2684,#2685,#565,.T.);
#3314=EDGE_CURVE('',#2685,#2683,#134,.T.);
#3315=EDGE_CURVE('',#2682,#2684,#135,.T.);
#3316=EDGE_CURVE('',#2686,#2687,#566,.T.);
#3317=EDGE_CURVE('',#2687,#2685,#136,.T.);
#3318=EDGE_CURVE('',#2684,#2686,#137,.T.);
#3319=EDGE_CURVE('',#2688,#2689,#567,.T.);
#3320=EDGE_CURVE('',#2689,#2687,#138,.T.);
#3321=EDGE_CURVE('',#2686,#2688,#139,.T.);
#3322=EDGE_CURVE('',#2690,#2691,#568,.T.);
#3323=EDGE_CURVE('',#2691,#2689,#140,.T.);
#3324=EDGE_CURVE('',#2688,#2690,#141,.T.);
#3325=EDGE_CURVE('',#2692,#2693,#569,.T.);
#3326=EDGE_CURVE('',#2693,#2691,#142,.T.);
#3327=EDGE_CURVE('',#2690,#2692,#143,.T.);
#3328=EDGE_CURVE('',#2694,#2695,#570,.T.);
#3329=EDGE_CURVE('',#2695,#2693,#144,.T.);
#3330=EDGE_CURVE('',#2692,#2694,#145,.T.);
#3331=EDGE_CURVE('',#2696,#2697,#571,.T.);
#3332=EDGE_CURVE('',#2697,#2695,#146,.T.);
#3333=EDGE_CURVE('',#2694,#2696,#147,.T.);
#3334=EDGE_CURVE('',#2698,#2699,#572,.T.);
#3335=EDGE_CURVE('',#2699,#2697,#148,.T.);
#3336=EDGE_CURVE('',#2696,#2698,#149,.T.);
#3337=EDGE_CURVE('',#2700,#2701,#573,.T.);
#3338=EDGE_CURVE('',#2701,#2699,#150,.T.);
#3339=EDGE_CURVE('',#2698,#2700,#151,.T.);
#3340=EDGE_CURVE('',#2702,#2703,#574,.T.);
#3341=EDGE_CURVE('',#2703,#2701,#152,.T.);
#3342=EDGE_CURVE('',#2700,#2702,#153,.T.);
#3343=EDGE_CURVE('',#2704,#2705,#575,.T.);
#3344=EDGE_CURVE('',#2705,#2703,#154,.T.);
#3345=EDGE_CURVE('',#2702,#2704,#155,.T.);
#3346=EDGE_CURVE('',#2706,#2707,#576,.T.);
#3347=EDGE_CURVE('',#2706,#2708,#156,.T.);
#3348=EDGE_CURVE('',#2709,#2708,#2492,.T.);
#3349=EDGE_CURVE('',#2709,#2707,#157,.T.);
#3350=EDGE_CURVE('',#2710,#2711,#577,.T.);
#3351=EDGE_CURVE('',#2711,#2712,#158,.T.);
#3352=EDGE_CURVE('',#2713,#2712,#2493,.T.);
#3353=EDGE_CURVE('',#2710,#2713,#159,.T.);
#3354=EDGE_CURVE('',#2714,#2715,#578,.T.);
#3355=EDGE_CURVE('',#2715,#2711,#160,.T.);
#3356=EDGE_CURVE('',#2714,#2710,#161,.T.);
#3357=EDGE_CURVE('',#2716,#2717,#579,.T.);
#3358=EDGE_CURVE('',#2717,#2715,#162,.T.);
#3359=EDGE_CURVE('',#2716,#2714,#163,.T.);
#3360=EDGE_CURVE('',#2718,#2719,#580,.T.);
#3361=EDGE_CURVE('',#2719,#2717,#164,.T.);
#3362=EDGE_CURVE('',#2718,#2716,#165,.T.);
#3363=EDGE_CURVE('',#2720,#2721,#581,.T.);
#3364=EDGE_CURVE('',#2721,#2719,#166,.T.);
#3365=EDGE_CURVE('',#2720,#2718,#167,.T.);
#3366=EDGE_CURVE('',#2722,#2723,#582,.T.);
#3367=EDGE_CURVE('',#2723,#2721,#168,.T.);
#3368=EDGE_CURVE('',#2722,#2720,#169,.T.);
#3369=EDGE_CURVE('',#2724,#2725,#583,.T.);
#3370=EDGE_CURVE('',#2725,#2723,#170,.T.);
#3371=EDGE_CURVE('',#2724,#2722,#171,.T.);
#3372=EDGE_CURVE('',#2726,#2727,#584,.T.);
#3373=EDGE_CURVE('',#2727,#2725,#172,.T.);
#3374=EDGE_CURVE('',#2726,#2724,#173,.T.);
#3375=EDGE_CURVE('',#2728,#2729,#585,.T.);
#3376=EDGE_CURVE('',#2729,#2727,#174,.T.);
#3377=EDGE_CURVE('',#2728,#2726,#175,.T.);
#3378=EDGE_CURVE('',#2730,#2731,#586,.T.);
#3379=EDGE_CURVE('',#2731,#2729,#176,.T.);
#3380=EDGE_CURVE('',#2730,#2728,#177,.T.);
#3381=EDGE_CURVE('',#2732,#2733,#587,.T.);
#3382=EDGE_CURVE('',#2733,#2731,#178,.T.);
#3383=EDGE_CURVE('',#2732,#2730,#179,.T.);
#3384=EDGE_CURVE('',#2734,#2735,#588,.T.);
#3385=EDGE_CURVE('',#2735,#2733,#180,.T.);
#3386=EDGE_CURVE('',#2734,#2732,#181,.T.);
#3387=EDGE_CURVE('',#2736,#2737,#589,.T.);
#3388=EDGE_CURVE('',#2737,#2735,#182,.T.);
#3389=EDGE_CURVE('',#2736,#2734,#183,.T.);
#3390=EDGE_CURVE('',#2738,#2739,#590,.T.);
#3391=EDGE_CURVE('',#2739,#2737,#184,.T.);
#3392=EDGE_CURVE('',#2738,#2736,#185,.T.);
#3393=EDGE_CURVE('',#2740,#2741,#591,.T.);
#3394=EDGE_CURVE('',#2741,#2739,#186,.T.);
#3395=EDGE_CURVE('',#2740,#2738,#187,.T.);
#3396=EDGE_CURVE('',#2742,#2743,#592,.T.);
#3397=EDGE_CURVE('',#2744,#2742,#188,.T.);
#3398=EDGE_CURVE('',#2745,#2744,#2494,.T.);
#3399=EDGE_CURVE('',#2745,#2743,#189,.T.);
#3400=EDGE_CURVE('',#2746,#2747,#593,.T.);
#3401=EDGE_CURVE('',#2747,#2748,#190,.T.);
#3402=EDGE_CURVE('',#2748,#2749,#2495,.T.);
#3403=EDGE_CURVE('',#2749,#2750,#191,.T.);
#3404=EDGE_CURVE('',#2750,#2751,#594,.T.);
#3405=EDGE_CURVE('',#2751,#2751,#2496,.F.);
#3406=EDGE_CURVE('',#2750,#2746,#192,.T.);
#3407=EDGE_CURVE('',#2752,#2753,#595,.T.);
#3408=EDGE_CURVE('',#2753,#2747,#193,.T.);
#3409=EDGE_CURVE('',#2746,#2752,#194,.T.);
#3410=EDGE_CURVE('',#2754,#2755,#596,.T.);
#3411=EDGE_CURVE('',#2755,#2753,#195,.T.);
#3412=EDGE_CURVE('',#2752,#2754,#196,.T.);
#3413=EDGE_CURVE('',#2756,#2757,#597,.T.);
#3414=EDGE_CURVE('',#2757,#2755,#197,.T.);
#3415=EDGE_CURVE('',#2754,#2756,#198,.T.);
#3416=EDGE_CURVE('',#2758,#2759,#598,.T.);
#3417=EDGE_CURVE('',#2759,#2757,#199,.T.);
#3418=EDGE_CURVE('',#2756,#2758,#200,.T.);
#3419=EDGE_CURVE('',#2760,#2761,#599,.T.);
#3420=EDGE_CURVE('',#2761,#2759,#201,.T.);
#3421=EDGE_CURVE('',#2758,#2760,#202,.T.);
#3422=EDGE_CURVE('',#2762,#2763,#600,.T.);
#3423=EDGE_CURVE('',#2763,#2761,#203,.T.);
#3424=EDGE_CURVE('',#2760,#2762,#204,.T.);
#3425=EDGE_CURVE('',#2764,#2765,#601,.T.);
#3426=EDGE_CURVE('',#2765,#2763,#205,.T.);
#3427=EDGE_CURVE('',#2762,#2764,#206,.T.);
#3428=EDGE_CURVE('',#2766,#2767,#602,.T.);
#3429=EDGE_CURVE('',#2767,#2765,#207,.T.);
#3430=EDGE_CURVE('',#2764,#2766,#208,.T.);
#3431=EDGE_CURVE('',#2768,#2769,#603,.T.);
#3432=EDGE_CURVE('',#2769,#2767,#209,.T.);
#3433=EDGE_CURVE('',#2766,#2768,#210,.T.);
#3434=EDGE_CURVE('',#2770,#2771,#604,.T.);
#3435=EDGE_CURVE('',#2771,#2769,#211,.T.);
#3436=EDGE_CURVE('',#2768,#2770,#212,.T.);
#3437=EDGE_CURVE('',#2772,#2773,#605,.T.);
#3438=EDGE_CURVE('',#2773,#2771,#213,.T.);
#3439=EDGE_CURVE('',#2770,#2772,#214,.T.);
#3440=EDGE_CURVE('',#2774,#2775,#606,.T.);
#3441=EDGE_CURVE('',#2775,#2773,#215,.T.);
#3442=EDGE_CURVE('',#2772,#2774,#216,.T.);
#3443=EDGE_CURVE('',#2776,#2777,#607,.T.);
#3444=EDGE_CURVE('',#2777,#2775,#217,.T.);
#3445=EDGE_CURVE('',#2774,#2776,#218,.T.);
#3446=EDGE_CURVE('',#2778,#2779,#608,.T.);
#3447=EDGE_CURVE('',#2778,#2780,#219,.T.);
#3448=EDGE_CURVE('',#2781,#2780,#2497,.T.);
#3449=EDGE_CURVE('',#2781,#2779,#220,.T.);
#3450=EDGE_CURVE('',#2782,#2783,#609,.T.);
#3451=EDGE_CURVE('',#2783,#2784,#221,.T.);
#3452=EDGE_CURVE('',#2785,#2784,#2498,.T.);
#3453=EDGE_CURVE('',#2782,#2785,#222,.T.);
#3454=EDGE_CURVE('',#2786,#2787,#610,.T.);
#3455=EDGE_CURVE('',#2787,#2783,#223,.T.);
#3456=EDGE_CURVE('',#2786,#2782,#224,.T.);
#3457=EDGE_CURVE('',#2788,#2789,#611,.T.);
#3458=EDGE_CURVE('',#2789,#2787,#225,.T.);
#3459=EDGE_CURVE('',#2788,#2786,#226,.T.);
#3460=EDGE_CURVE('',#2790,#2791,#612,.T.);
#3461=EDGE_CURVE('',#2791,#2789,#227,.T.);
#3462=EDGE_CURVE('',#2790,#2788,#228,.T.);
#3463=EDGE_CURVE('',#2792,#2793,#613,.T.);
#3464=EDGE_CURVE('',#2793,#2791,#229,.T.);
#3465=EDGE_CURVE('',#2792,#2790,#230,.T.);
#3466=EDGE_CURVE('',#2794,#2795,#614,.T.);
#3467=EDGE_CURVE('',#2795,#2793,#231,.T.);
#3468=EDGE_CURVE('',#2794,#2792,#232,.T.);
#3469=EDGE_CURVE('',#2796,#2797,#615,.T.);
#3470=EDGE_CURVE('',#2797,#2795,#233,.T.);
#3471=EDGE_CURVE('',#2796,#2794,#234,.T.);
#3472=EDGE_CURVE('',#2798,#2799,#616,.T.);
#3473=EDGE_CURVE('',#2799,#2797,#235,.T.);
#3474=EDGE_CURVE('',#2798,#2796,#236,.T.);
#3475=EDGE_CURVE('',#2800,#2801,#617,.T.);
#3476=EDGE_CURVE('',#2801,#2799,#237,.T.);
#3477=EDGE_CURVE('',#2800,#2798,#238,.T.);
#3478=EDGE_CURVE('',#2802,#2803,#618,.T.);
#3479=EDGE_CURVE('',#2803,#2801,#239,.T.);
#3480=EDGE_CURVE('',#2802,#2800,#240,.T.);
#3481=EDGE_CURVE('',#2804,#2805,#619,.T.);
#3482=EDGE_CURVE('',#2805,#2803,#241,.T.);
#3483=EDGE_CURVE('',#2804,#2802,#242,.T.);
#3484=EDGE_CURVE('',#2806,#2807,#620,.T.);
#3485=EDGE_CURVE('',#2807,#2805,#243,.T.);
#3486=EDGE_CURVE('',#2806,#2804,#244,.T.);
#3487=EDGE_CURVE('',#2808,#2809,#621,.T.);
#3488=EDGE_CURVE('',#2809,#2807,#245,.T.);
#3489=EDGE_CURVE('',#2808,#2806,#246,.T.);
#3490=EDGE_CURVE('',#2810,#2811,#622,.T.);
#3491=EDGE_CURVE('',#2811,#2809,#247,.T.);
#3492=EDGE_CURVE('',#2810,#2808,#248,.T.);
#3493=EDGE_CURVE('',#2812,#2813,#623,.T.);
#3494=EDGE_CURVE('',#2813,#2811,#249,.T.);
#3495=EDGE_CURVE('',#2812,#2810,#250,.T.);
#3496=EDGE_CURVE('',#2814,#2815,#624,.T.);
#3497=EDGE_CURVE('',#2816,#2814,#251,.T.);
#3498=EDGE_CURVE('',#2817,#2816,#2499,.T.);
#3499=EDGE_CURVE('',#2817,#2815,#252,.T.);
#3500=EDGE_CURVE('',#2748,#2785,#253,.T.);
#3501=EDGE_CURVE('',#2784,#2749,#254,.T.);
#3502=EDGE_CURVE('',#2815,#2813,#255,.T.);
#3503=EDGE_CURVE('',#2814,#2812,#256,.T.);
#3504=EDGE_CURVE('',#2780,#2817,#257,.T.);
#3505=EDGE_CURVE('',#2776,#2778,#258,.T.);
#3506=EDGE_CURVE('',#2779,#2777,#259,.T.);
#3507=EDGE_CURVE('',#2816,#2781,#260,.T.);
#3508=EDGE_CURVE('',#2676,#2713,#261,.T.);
#3509=EDGE_CURVE('',#2712,#2677,#262,.T.);
#3510=EDGE_CURVE('',#2743,#2741,#263,.T.);
#3511=EDGE_CURVE('',#2742,#2740,#264,.T.);
#3512=EDGE_CURVE('',#2708,#2745,#265,.T.);
#3513=EDGE_CURVE('',#2704,#2706,#266,.T.);
#3514=EDGE_CURVE('',#2707,#2705,#267,.T.);
#3515=EDGE_CURVE('',#2744,#2709,#268,.T.);
#3516=EDGE_CURVE('',#2818,#2818,#2500,.T.);
#3517=EDGE_CURVE('',#2818,#2819,#625,.T.);
#3518=EDGE_CURVE('',#2819,#2819,#2501,.T.);
#3519=EDGE_CURVE('',#2820,#2820,#2502,.T.);
#3520=EDGE_CURVE('',#2820,#2821,#626,.T.);
#3521=EDGE_CURVE('',#2821,#2821,#2503,.T.);
#3522=EDGE_CURVE('',#2822,#2822,#2504,.T.);
#3523=EDGE_CURVE('',#2822,#2823,#627,.T.);
#3524=EDGE_CURVE('',#2823,#2823,#2505,.T.);
#3525=EDGE_CURVE('',#2824,#2825,#628,.T.);
#3526=EDGE_CURVE('',#2826,#2824,#629,.T.);
#3527=EDGE_CURVE('',#2826,#2827,#630,.T.);
#3528=EDGE_CURVE('',#2827,#2825,#631,.T.);
#3529=EDGE_CURVE('',#2828,#2829,#632,.T.);
#3530=EDGE_CURVE('',#2830,#2828,#633,.T.);
#3531=EDGE_CURVE('',#2830,#2831,#634,.T.);
#3532=EDGE_CURVE('',#2831,#2829,#635,.T.);
#3533=EDGE_CURVE('',#2831,#2826,#636,.T.);
#3534=EDGE_CURVE('',#2827,#2830,#637,.T.);
#3535=EDGE_CURVE('',#2832,#2825,#638,.T.);
#3536=EDGE_CURVE('',#2833,#2832,#639,.T.);
#3537=EDGE_CURVE('',#2824,#2833,#640,.T.);
#3538=EDGE_CURVE('',#2834,#2829,#641,.T.);
#3539=EDGE_CURVE('',#2835,#2834,#642,.T.);
#3540=EDGE_CURVE('',#2828,#2835,#643,.T.);
#3541=EDGE_CURVE('',#2836,#2837,#644,.T.);
#3542=EDGE_CURVE('',#2838,#2836,#645,.T.);
#3543=EDGE_CURVE('',#2838,#2839,#646,.T.);
#3544=EDGE_CURVE('',#2839,#2837,#647,.T.);
#3545=EDGE_CURVE('',#2840,#2836,#648,.T.);
#3546=EDGE_CURVE('',#2841,#2840,#649,.T.);
#3547=EDGE_CURVE('',#2841,#2838,#650,.T.);
#3548=EDGE_CURVE('',#2837,#2842,#651,.T.);
#3549=EDGE_CURVE('',#2839,#2843,#652,.T.);
#3550=EDGE_CURVE('',#2843,#2842,#653,.T.);
#3551=EDGE_CURVE('',#2843,#2841,#654,.T.);
#3552=EDGE_CURVE('',#2844,#2842,#655,.T.);
#3553=EDGE_CURVE('',#2845,#2844,#656,.T.);
#3554=EDGE_CURVE('',#2846,#2845,#657,.T.);
#3555=EDGE_CURVE('',#2846,#2847,#658,.T.);
#3556=EDGE_CURVE('',#2847,#2848,#659,.T.);
#3557=EDGE_CURVE('',#2848,#2849,#660,.T.);
#3558=EDGE_CURVE('',#2850,#2849,#661,.T.);
#3559=EDGE_CURVE('',#2851,#2850,#662,.T.);
#3560=EDGE_CURVE('',#2840,#2851,#663,.T.);
#3561=EDGE_CURVE('',#2852,#2853,#664,.T.);
#3562=EDGE_CURVE('',#2853,#2854,#665,.T.);
#3563=EDGE_CURVE('',#2854,#2855,#666,.T.);
#3564=EDGE_CURVE('',#2855,#2852,#667,.T.);
#3565=EDGE_CURVE('',#2856,#2857,#668,.T.);
#3566=EDGE_CURVE('',#2857,#2858,#669,.T.);
#3567=EDGE_CURVE('',#2858,#2859,#670,.T.);
#3568=EDGE_CURVE('',#2859,#2856,#671,.T.);
#3569=EDGE_CURVE('',#2833,#2848,#672,.T.);
#3570=EDGE_CURVE('',#2834,#2847,#673,.T.);
#3571=EDGE_CURVE('',#2835,#2846,#674,.T.);
#3572=EDGE_CURVE('',#2832,#2849,#675,.T.);
#3573=EDGE_CURVE('',#2845,#2860,#676,.T.);
#3574=EDGE_CURVE('',#2861,#2860,#677,.T.);
#3575=EDGE_CURVE('',#2861,#2862,#678,.T.);
#3576=EDGE_CURVE('',#2862,#2863,#679,.T.);
#3577=EDGE_CURVE('',#2863,#2864,#680,.T.);
#3578=EDGE_CURVE('',#2865,#2864,#681,.T.);
#3579=EDGE_CURVE('',#2850,#2865,#682,.T.);
#3580=EDGE_CURVE('',#2866,#2867,#683,.T.);
#3581=EDGE_CURVE('',#2866,#2857,#684,.T.);
#3582=EDGE_CURVE('',#2867,#2856,#685,.T.);
#3583=EDGE_CURVE('',#2868,#2866,#686,.T.);
#3584=EDGE_CURVE('',#2868,#2858,#687,.T.);
#3585=EDGE_CURVE('',#2869,#2868,#688,.T.);
#3586=EDGE_CURVE('',#2869,#2859,#689,.T.);
#3587=EDGE_CURVE('',#2867,#2869,#690,.T.);
#3588=EDGE_CURVE('',#2870,#2871,#691,.T.);
#3589=EDGE_CURVE('',#2870,#2853,#692,.T.);
#3590=EDGE_CURVE('',#2871,#2852,#693,.T.);
#3591=EDGE_CURVE('',#2872,#2870,#694,.T.);
#3592=EDGE_CURVE('',#2872,#2854,#695,.T.);
#3593=EDGE_CURVE('',#2873,#2872,#696,.T.);
#3594=EDGE_CURVE('',#2873,#2855,#697,.T.);
#3595=EDGE_CURVE('',#2871,#2873,#698,.T.);
#3596=EDGE_CURVE('',#2874,#2875,#699,.T.);
#3597=EDGE_CURVE('',#2864,#2874,#700,.T.);
#3598=EDGE_CURVE('',#2863,#2876,#701,.T.);
#3599=EDGE_CURVE('',#2876,#2877,#702,.T.);
#3600=EDGE_CURVE('',#2878,#2877,#703,.T.);
#3601=EDGE_CURVE('',#2879,#2878,#704,.T.);
#3602=EDGE_CURVE('',#2879,#2875,#705,.T.);
#3603=EDGE_CURVE('',#2880,#2862,#706,.T.);
#3604=EDGE_CURVE('',#2876,#2880,#707,.T.);
#3605=EDGE_CURVE('',#2875,#2881,#708,.T.);
#3606=EDGE_CURVE('',#2882,#2879,#709,.T.);
#3607=EDGE_CURVE('',#2881,#2882,#710,.T.);
#3608=EDGE_CURVE('',#2883,#2878,#711,.T.);
#3609=EDGE_CURVE('',#2882,#2883,#712,.T.);
#3610=EDGE_CURVE('',#2881,#2884,#713,.T.);
#3611=EDGE_CURVE('',#2885,#2883,#714,.T.);
#3612=EDGE_CURVE('',#2880,#2885,#715,.T.);
#3613=EDGE_CURVE('',#2884,#2861,#716,.T.);
#3614=EDGE_CURVE('',#2877,#2885,#717,.T.);
#3615=EDGE_CURVE('',#2874,#2886,#718,.T.);
#3616=EDGE_CURVE('',#2886,#2865,#719,.T.);
#3617=EDGE_CURVE('',#2860,#2887,#720,.T.);
#3618=EDGE_CURVE('',#2887,#2884,#721,.T.);
#3619=EDGE_CURVE('',#2851,#2886,#722,.T.);
#3620=EDGE_CURVE('',#2844,#2887,#723,.T.);
#3621=EDGE_CURVE('',#2888,#2889,#724,.T.);
#3622=EDGE_CURVE('',#2889,#2890,#269,.T.);
#3623=EDGE_CURVE('',#2891,#2890,#2506,.F.);
#3624=EDGE_CURVE('',#2891,#2888,#270,.T.);
#3625=EDGE_CURVE('',#2892,#2893,#725,.T.);
#3626=EDGE_CURVE('',#2893,#2889,#271,.T.);
#3627=EDGE_CURVE('',#2888,#2892,#272,.T.);
#3628=EDGE_CURVE('',#2894,#2895,#726,.T.);
#3629=EDGE_CURVE('',#2895,#2893,#273,.T.);
#3630=EDGE_CURVE('',#2892,#2894,#274,.T.);
#3631=EDGE_CURVE('',#2896,#2897,#727,.T.);
#3632=EDGE_CURVE('',#2897,#2895,#275,.T.);
#3633=EDGE_CURVE('',#2894,#2896,#276,.T.);
#3634=EDGE_CURVE('',#2898,#2899,#728,.T.);
#3635=EDGE_CURVE('',#2899,#2897,#277,.T.);
#3636=EDGE_CURVE('',#2896,#2898,#278,.T.);
#3637=EDGE_CURVE('',#2900,#2901,#729,.T.);
#3638=EDGE_CURVE('',#2901,#2899,#279,.T.);
#3639=EDGE_CURVE('',#2898,#2900,#280,.T.);
#3640=EDGE_CURVE('',#2902,#2903,#730,.T.);
#3641=EDGE_CURVE('',#2903,#2901,#281,.T.);
#3642=EDGE_CURVE('',#2900,#2902,#282,.T.);
#3643=EDGE_CURVE('',#2904,#2905,#731,.T.);
#3644=EDGE_CURVE('',#2905,#2903,#283,.T.);
#3645=EDGE_CURVE('',#2902,#2904,#284,.T.);
#3646=EDGE_CURVE('',#2906,#2907,#732,.T.);
#3647=EDGE_CURVE('',#2907,#2905,#285,.T.);
#3648=EDGE_CURVE('',#2904,#2906,#286,.T.);
#3649=EDGE_CURVE('',#2908,#2909,#733,.T.);
#3650=EDGE_CURVE('',#2908,#2910,#287,.T.);
#3651=EDGE_CURVE('',#2911,#2910,#2507,.T.);
#3652=EDGE_CURVE('',#2911,#2909,#288,.T.);
#3653=EDGE_CURVE('',#2912,#2913,#734,.T.);
#3654=EDGE_CURVE('',#2913,#2914,#289,.T.);
#3655=EDGE_CURVE('',#2915,#2914,#2508,.T.);
#3656=EDGE_CURVE('',#2912,#2915,#290,.T.);
#3657=EDGE_CURVE('',#2916,#2917,#735,.T.);
#3658=EDGE_CURVE('',#2917,#2913,#291,.T.);
#3659=EDGE_CURVE('',#2916,#2912,#292,.T.);
#3660=EDGE_CURVE('',#2918,#2919,#736,.T.);
#3661=EDGE_CURVE('',#2919,#2917,#293,.T.);
#3662=EDGE_CURVE('',#2918,#2916,#294,.T.);
#3663=EDGE_CURVE('',#2920,#2921,#737,.T.);
#3664=EDGE_CURVE('',#2921,#2919,#295,.T.);
#3665=EDGE_CURVE('',#2920,#2918,#296,.T.);
#3666=EDGE_CURVE('',#2922,#2923,#738,.T.);
#3667=EDGE_CURVE('',#2923,#2921,#297,.T.);
#3668=EDGE_CURVE('',#2922,#2920,#298,.T.);
#3669=EDGE_CURVE('',#2924,#2925,#739,.T.);
#3670=EDGE_CURVE('',#2925,#2923,#299,.T.);
#3671=EDGE_CURVE('',#2924,#2922,#300,.T.);
#3672=EDGE_CURVE('',#2926,#2927,#740,.T.);
#3673=EDGE_CURVE('',#2927,#2925,#301,.T.);
#3674=EDGE_CURVE('',#2926,#2924,#302,.T.);
#3675=EDGE_CURVE('',#2928,#2929,#741,.T.);
#3676=EDGE_CURVE('',#2929,#2927,#303,.T.);
#3677=EDGE_CURVE('',#2928,#2926,#304,.T.);
#3678=EDGE_CURVE('',#2930,#2931,#742,.T.);
#3679=EDGE_CURVE('',#2931,#2929,#305,.T.);
#3680=EDGE_CURVE('',#2930,#2928,#306,.T.);
#3681=EDGE_CURVE('',#2932,#2933,#743,.T.);
#3682=EDGE_CURVE('',#2934,#2932,#307,.T.);
#3683=EDGE_CURVE('',#2935,#2934,#2509,.T.);
#3684=EDGE_CURVE('',#2935,#2933,#308,.T.);
#3685=EDGE_CURVE('',#2936,#2937,#2510,.T.);
#3686=EDGE_CURVE('',#2936,#2938,#744,.T.);
#3687=EDGE_CURVE('',#2939,#2938,#2511,.T.);
#3688=EDGE_CURVE('',#2937,#2939,#745,.T.);
#3689=EDGE_CURVE('',#2940,#2936,#2512,.T.);
#3690=EDGE_CURVE('',#2940,#2941,#746,.T.);
#3691=EDGE_CURVE('',#2938,#2941,#2513,.T.);
#3692=EDGE_CURVE('',#2942,#2940,#2514,.T.);
#3693=EDGE_CURVE('',#2942,#2943,#747,.T.);
#3694=EDGE_CURVE('',#2941,#2943,#2515,.T.);
#3695=EDGE_CURVE('',#2937,#2942,#2516,.T.);
#3696=EDGE_CURVE('',#2943,#2939,#2517,.T.);
#3697=EDGE_CURVE('',#2933,#2931,#309,.T.);
#3698=EDGE_CURVE('',#2932,#2930,#310,.T.);
#3699=EDGE_CURVE('',#2914,#2891,#311,.T.);
#3700=EDGE_CURVE('',#2910,#2935,#312,.T.);
#3701=EDGE_CURVE('',#2906,#2908,#313,.T.);
#3702=EDGE_CURVE('',#2890,#2915,#314,.T.);
#3703=EDGE_CURVE('',#2909,#2907,#315,.T.);
#3704=EDGE_CURVE('',#2934,#2911,#316,.T.);
#3705=EDGE_CURVE('',#2944,#2944,#2518,.T.);
#3706=EDGE_CURVE('',#2945,#2945,#2519,.T.);
#3707=EDGE_CURVE('',#2945,#2946,#748,.T.);
#3708=EDGE_CURVE('',#2946,#2946,#2520,.T.);
#3709=EDGE_CURVE('',#2947,#2947,#2521,.T.);
#3710=EDGE_CURVE('',#2947,#2948,#749,.T.);
#3711=EDGE_CURVE('',#2948,#2948,#2522,.T.);
#3712=EDGE_CURVE('',#2949,#2949,#2523,.T.);
#3713=EDGE_CURVE('',#2949,#2950,#750,.T.);
#3714=EDGE_CURVE('',#2950,#2950,#2524,.T.);
#3715=EDGE_CURVE('',#2944,#2951,#751,.T.);
#3716=EDGE_CURVE('',#2951,#2951,#2525,.T.);
#3717=EDGE_CURVE('',#2952,#2953,#752,.T.);
#3718=EDGE_CURVE('',#2952,#2954,#2526,.T.);
#3719=EDGE_CURVE('',#2954,#2955,#753,.T.);
#3720=EDGE_CURVE('',#2953,#2955,#2527,.T.);
#3721=EDGE_CURVE('',#2955,#2956,#754,.T.);
#3722=EDGE_CURVE('',#2956,#2957,#755,.T.);
#3723=EDGE_CURVE('',#2957,#2958,#2528,.T.);
#3724=EDGE_CURVE('',#2958,#2959,#756,.T.);
#3725=EDGE_CURVE('',#2959,#2960,#2529,.T.);
#3726=EDGE_CURVE('',#2960,#2961,#757,.T.);
#3727=EDGE_CURVE('',#2961,#2962,#2530,.T.);
#3728=EDGE_CURVE('',#2962,#2963,#758,.T.);
#3729=EDGE_CURVE('',#2963,#2953,#759,.T.);
#3730=EDGE_CURVE('',#2964,#2963,#760,.T.);
#3731=EDGE_CURVE('',#2964,#2952,#761,.T.);
#3732=EDGE_CURVE('',#2956,#2965,#762,.T.);
#3733=EDGE_CURVE('',#2954,#2965,#763,.T.);
#3734=EDGE_CURVE('',#2965,#2966,#764,.T.);
#3735=EDGE_CURVE('',#2966,#2957,#765,.T.);
#3736=EDGE_CURVE('',#2967,#2964,#766,.T.);
#3737=EDGE_CURVE('',#2968,#2967,#2531,.T.);
#3738=EDGE_CURVE('',#2969,#2968,#767,.T.);
#3739=EDGE_CURVE('',#2970,#2969,#2532,.T.);
#3740=EDGE_CURVE('',#2971,#2970,#768,.T.);
#3741=EDGE_CURVE('',#2966,#2971,#2533,.T.);
#3742=EDGE_CURVE('',#2960,#2969,#769,.T.);
#3743=EDGE_CURVE('',#2970,#2959,#770,.T.);
#3744=EDGE_CURVE('',#2967,#2962,#771,.T.);
#3745=EDGE_CURVE('',#2971,#2958,#772,.T.);
#3746=EDGE_CURVE('',#2968,#2961,#773,.T.);
#3747=EDGE_CURVE('',#2972,#2973,#774,.T.);
#3748=EDGE_CURVE('',#2974,#2973,#775,.T.);
#3749=EDGE_CURVE('',#2974,#2975,#776,.T.);
#3750=EDGE_CURVE('',#2972,#2975,#777,.T.);
#3751=EDGE_CURVE('',#2976,#2974,#2534,.T.);
#3752=EDGE_CURVE('',#2976,#2977,#778,.T.);
#3753=EDGE_CURVE('',#2975,#2977,#2535,.T.);
#3754=EDGE_CURVE('',#2978,#2976,#779,.T.);
#3755=EDGE_CURVE('',#2978,#2979,#780,.T.);
#3756=EDGE_CURVE('',#2977,#2979,#781,.T.);
#3757=EDGE_CURVE('',#2973,#2978,#2536,.T.);
#3758=EDGE_CURVE('',#2979,#2972,#2537,.T.);
#3759=EDGE_CURVE('',#2980,#2981,#782,.T.);
#3760=EDGE_CURVE('',#2982,#2981,#783,.T.);
#3761=EDGE_CURVE('',#2983,#2982,#784,.T.);
#3762=EDGE_CURVE('',#2980,#2983,#785,.T.);
#3763=EDGE_CURVE('',#2984,#2985,#786,.T.);
#3764=EDGE_CURVE('',#2986,#2985,#787,.T.);
#3765=EDGE_CURVE('',#2987,#2986,#788,.T.);
#3766=EDGE_CURVE('',#2984,#2987,#789,.T.);
#3767=EDGE_CURVE('',#2986,#2988,#790,.T.);
#3768=EDGE_CURVE('',#2989,#2988,#791,.T.);
#3769=EDGE_CURVE('',#2987,#2989,#792,.T.);
#3770=EDGE_CURVE('',#2984,#2981,#793,.T.);
#3771=EDGE_CURVE('',#2990,#2989,#794,.T.);
#3772=EDGE_CURVE('',#2982,#2990,#795,.T.);
#3773=EDGE_CURVE('',#2991,#2990,#796,.T.);
#3774=EDGE_CURVE('',#2983,#2991,#797,.T.);
#3775=EDGE_CURVE('',#2980,#2985,#798,.T.);
#3776=EDGE_CURVE('',#2988,#2991,#799,.T.);
#3777=EDGE_CURVE('',#2985,#2992,#800,.T.);
#3778=EDGE_CURVE('',#2992,#2993,#801,.T.);
#3779=EDGE_CURVE('',#2993,#2980,#802,.T.);
#3780=EDGE_CURVE('',#2981,#2994,#803,.T.);
#3781=EDGE_CURVE('',#2994,#2995,#804,.T.);
#3782=EDGE_CURVE('',#2995,#2984,#805,.T.);
#3783=EDGE_CURVE('',#2996,#2997,#806,.T.);
#3784=EDGE_CURVE('',#2996,#2995,#807,.T.);
#3785=EDGE_CURVE('',#2997,#2994,#808,.T.);
#3786=EDGE_CURVE('',#2998,#2999,#809,.T.);
#3787=EDGE_CURVE('',#2998,#2993,#810,.T.);
#3788=EDGE_CURVE('',#2999,#2992,#811,.T.);
#3789=EDGE_CURVE('',#2999,#3000,#812,.T.);
#3790=EDGE_CURVE('',#3000,#3001,#813,.T.);
#3791=EDGE_CURVE('',#3001,#2998,#814,.T.);
#3792=EDGE_CURVE('',#3002,#3003,#815,.T.);
#3793=EDGE_CURVE('',#3003,#3000,#816,.T.);
#3794=EDGE_CURVE('',#3004,#2996,#817,.T.);
#3795=EDGE_CURVE('',#3002,#3004,#818,.T.);
#3796=EDGE_CURVE('',#3005,#3002,#819,.T.);
#3797=EDGE_CURVE('',#3006,#3004,#820,.T.);
#3798=EDGE_CURVE('',#3005,#3006,#821,.T.);
#3799=EDGE_CURVE('',#3007,#3005,#822,.T.);
#3800=EDGE_CURVE('',#2997,#3006,#823,.T.);
#3801=EDGE_CURVE('',#3007,#3001,#824,.T.);
#3802=EDGE_CURVE('',#3003,#3007,#825,.T.);
#3803=EDGE_CURVE('',#3008,#3008,#2538,.T.);
#3804=EDGE_CURVE('',#3008,#3009,#826,.T.);
#3805=EDGE_CURVE('',#3009,#3009,#2539,.T.);
#3806=EDGE_CURVE('',#3010,#3010,#2540,.T.);
#3807=EDGE_CURVE('',#3011,#3011,#2541,.T.);
#3808=EDGE_CURVE('',#3012,#3012,#2542,.T.);
#3809=EDGE_CURVE('',#3012,#3011,#827,.T.);
#3810=EDGE_CURVE('',#3013,#3013,#2543,.T.);
#3811=EDGE_CURVE('',#3014,#3014,#2544,.T.);
#3812=EDGE_CURVE('',#3013,#3015,#828,.T.);
#3813=EDGE_CURVE('',#3015,#3015,#2545,.T.);
#3814=EDGE_CURVE('',#3010,#3014,#829,.T.);
#3815=EDGE_CURVE('',#3016,#3016,#2546,.T.);
#3816=EDGE_CURVE('',#3016,#3017,#830,.T.);
#3817=EDGE_CURVE('',#3017,#3017,#2547,.T.);
#3818=EDGE_CURVE('',#3018,#3018,#2548,.T.);
#3819=EDGE_CURVE('',#3019,#3019,#2549,.T.);
#3820=EDGE_CURVE('',#3020,#3020,#2550,.T.);
#3821=EDGE_CURVE('',#3020,#3019,#831,.T.);
#3822=EDGE_CURVE('',#3021,#3021,#2551,.T.);
#3823=EDGE_CURVE('',#3022,#3022,#2552,.T.);
#3824=EDGE_CURVE('',#3021,#3023,#832,.T.);
#3825=EDGE_CURVE('',#3023,#3023,#2553,.T.);
#3826=EDGE_CURVE('',#3018,#3022,#833,.T.);
#3827=EDGE_CURVE('',#3024,#3024,#2554,.T.);
#3828=EDGE_CURVE('',#3024,#3025,#834,.T.);
#3829=EDGE_CURVE('',#3025,#3025,#2555,.T.);
#3830=EDGE_CURVE('',#3026,#3026,#2556,.T.);
#3831=EDGE_CURVE('',#3026,#3027,#835,.T.);
#3832=EDGE_CURVE('',#3027,#3027,#2557,.T.);
#3833=EDGE_CURVE('',#3028,#3029,#836,.T.);
#3834=EDGE_CURVE('',#3030,#3028,#837,.T.);
#3835=EDGE_CURVE('',#3031,#3030,#838,.T.);
#3836=EDGE_CURVE('',#3029,#3031,#839,.T.);
#3837=EDGE_CURVE('',#3032,#3033,#840,.T.);
#3838=EDGE_CURVE('',#3034,#3032,#841,.T.);
#3839=EDGE_CURVE('',#3035,#3034,#842,.T.);
#3840=EDGE_CURVE('',#3033,#3035,#843,.T.);
#3841=EDGE_CURVE('',#3030,#3035,#2558,.T.);
#3842=EDGE_CURVE('',#3033,#3028,#2559,.T.);
#3843=EDGE_CURVE('',#3032,#3029,#2560,.T.);
#3844=EDGE_CURVE('',#3031,#3034,#2561,.T.);
#3845=EDGE_CURVE('',#3036,#3036,#2562,.T.);
#3846=EDGE_CURVE('',#3036,#3037,#844,.T.);
#3847=EDGE_CURVE('',#3037,#3037,#2563,.T.);
#3848=EDGE_CURVE('',#3038,#3038,#2564,.T.);
#3849=EDGE_CURVE('',#3038,#3039,#845,.T.);
#3850=EDGE_CURVE('',#3039,#3039,#2565,.T.);
#3851=EDGE_CURVE('',#3040,#3040,#2566,.T.);
#3852=EDGE_CURVE('',#3040,#3041,#846,.T.);
#3853=EDGE_CURVE('',#3041,#3041,#2567,.T.);
#3854=EDGE_CURVE('',#3042,#3042,#2568,.T.);
#3855=EDGE_CURVE('',#3042,#3043,#847,.T.);
#3856=EDGE_CURVE('',#3043,#3043,#2569,.T.);
#3857=EDGE_CURVE('',#3044,#3044,#2570,.T.);
#3858=EDGE_CURVE('',#3044,#3045,#848,.T.);
#3859=EDGE_CURVE('',#3045,#3045,#2571,.T.);
#3860=EDGE_CURVE('',#3046,#3046,#2572,.T.);
#3861=EDGE_CURVE('',#3046,#3047,#849,.T.);
#3862=EDGE_CURVE('',#3047,#3047,#2573,.T.);
#3863=EDGE_CURVE('',#3048,#3049,#850,.T.);
#3864=EDGE_CURVE('',#3050,#3048,#851,.T.);
#3865=EDGE_CURVE('',#3051,#3050,#852,.T.);
#3866=EDGE_CURVE('',#3049,#3051,#853,.T.);
#3867=EDGE_CURVE('',#3052,#3053,#854,.T.);
#3868=EDGE_CURVE('',#3054,#3052,#855,.T.);
#3869=EDGE_CURVE('',#3055,#3054,#856,.T.);
#3870=EDGE_CURVE('',#3053,#3055,#857,.T.);
#3871=EDGE_CURVE('',#3050,#3055,#2574,.T.);
#3872=EDGE_CURVE('',#3053,#3048,#2575,.T.);
#3873=EDGE_CURVE('',#3052,#3049,#2576,.T.);
#3874=EDGE_CURVE('',#3051,#3054,#2577,.T.);
#3875=EDGE_CURVE('',#3056,#3056,#2578,.T.);
#3876=EDGE_CURVE('',#3056,#3057,#858,.T.);
#3877=EDGE_CURVE('',#3057,#3057,#2579,.T.);
#3878=EDGE_CURVE('',#3058,#3058,#2580,.T.);
#3879=EDGE_CURVE('',#3059,#3059,#2581,.T.);
#3880=EDGE_CURVE('',#3060,#3060,#2582,.T.);
#3881=EDGE_CURVE('',#3060,#3059,#859,.T.);
#3882=EDGE_CURVE('',#3061,#3061,#2583,.T.);
#3883=EDGE_CURVE('',#3062,#3062,#2584,.T.);
#3884=EDGE_CURVE('',#3061,#3063,#860,.T.);
#3885=EDGE_CURVE('',#3063,#3063,#2585,.T.);
#3886=EDGE_CURVE('',#3058,#3062,#861,.T.);
#3887=EDGE_CURVE('',#3064,#3064,#2586,.T.);
#3888=EDGE_CURVE('',#3064,#3065,#862,.T.);
#3889=EDGE_CURVE('',#3065,#3065,#2587,.T.);
#3890=EDGE_CURVE('',#3066,#3066,#2588,.T.);
#3891=EDGE_CURVE('',#3066,#3067,#863,.T.);
#3892=EDGE_CURVE('',#3067,#3067,#2589,.T.);
#3893=EDGE_CURVE('',#3068,#3068,#2590,.T.);
#3894=EDGE_CURVE('',#3068,#3069,#864,.T.);
#3895=EDGE_CURVE('',#3069,#3069,#2591,.T.);
#3896=EDGE_CURVE('',#3070,#3070,#2592,.T.);
#3897=EDGE_CURVE('',#3070,#3071,#865,.T.);
#3898=EDGE_CURVE('',#3071,#3071,#2593,.T.);
#3899=EDGE_CURVE('',#3072,#3073,#866,.T.);
#3900=EDGE_CURVE('',#3074,#3072,#867,.T.);
#3901=EDGE_CURVE('',#3075,#3074,#868,.T.);
#3902=EDGE_CURVE('',#3073,#3075,#869,.T.);
#3903=EDGE_CURVE('',#3076,#3077,#870,.T.);
#3904=EDGE_CURVE('',#3078,#3076,#871,.T.);
#3905=EDGE_CURVE('',#3079,#3078,#872,.T.);
#3906=EDGE_CURVE('',#3077,#3079,#873,.T.);
#3907=EDGE_CURVE('',#3074,#3079,#2594,.T.);
#3908=EDGE_CURVE('',#3077,#3072,#2595,.T.);
#3909=EDGE_CURVE('',#3076,#3073,#2596,.T.);
#3910=EDGE_CURVE('',#3075,#3078,#2597,.T.);
#3911=EDGE_CURVE('',#3080,#3080,#2598,.T.);
#3912=EDGE_CURVE('',#3080,#3081,#874,.T.);
#3913=EDGE_CURVE('',#3081,#3081,#2599,.T.);
#3914=EDGE_CURVE('',#3082,#3082,#2600,.F.);
#3915=EDGE_CURVE('',#3082,#3083,#875,.T.);
#3916=EDGE_CURVE('',#3083,#3083,#2601,.F.);
#3917=EDGE_CURVE('',#3084,#3085,#876,.T.);
#3918=EDGE_CURVE('',#3084,#3086,#317,.T.);
#3919=EDGE_CURVE('',#3087,#3086,#2602,.T.);
#3920=EDGE_CURVE('',#3085,#3087,#318,.T.);
#3921=EDGE_CURVE('',#3088,#3089,#877,.T.);
#3922=EDGE_CURVE('',#3088,#3084,#319,.T.);
#3923=EDGE_CURVE('',#3089,#3085,#320,.T.);
#3924=EDGE_CURVE('',#3090,#3091,#878,.T.);
#3925=EDGE_CURVE('',#3090,#3088,#321,.T.);
#3926=EDGE_CURVE('',#3091,#3089,#322,.T.);
#3927=EDGE_CURVE('',#3092,#3093,#879,.T.);
#3928=EDGE_CURVE('',#3092,#3090,#323,.T.);
#3929=EDGE_CURVE('',#3093,#3091,#324,.T.);
#3930=EDGE_CURVE('',#3094,#3095,#880,.T.);
#3931=EDGE_CURVE('',#3094,#3092,#325,.T.);
#3932=EDGE_CURVE('',#3095,#3093,#326,.T.);
#3933=EDGE_CURVE('',#3096,#3097,#881,.T.);
#3934=EDGE_CURVE('',#3096,#3094,#327,.T.);
#3935=EDGE_CURVE('',#3097,#3095,#328,.T.);
#3936=EDGE_CURVE('',#3098,#3099,#882,.T.);
#3937=EDGE_CURVE('',#3098,#3096,#329,.T.);
#3938=EDGE_CURVE('',#3099,#3097,#330,.T.);
#3939=EDGE_CURVE('',#3100,#3101,#883,.T.);
#3940=EDGE_CURVE('',#3100,#3098,#331,.T.);
#3941=EDGE_CURVE('',#3101,#3099,#332,.T.);
#3942=EDGE_CURVE('',#3102,#3103,#884,.T.);
#3943=EDGE_CURVE('',#3102,#3104,#333,.T.);
#3944=EDGE_CURVE('',#3104,#3105,#2603,.T.);
#3945=EDGE_CURVE('',#3105,#3103,#334,.T.);
#3946=EDGE_CURVE('',#3106,#3107,#885,.T.);
#3947=EDGE_CURVE('',#3106,#3102,#335,.T.);
#3948=EDGE_CURVE('',#3103,#3107,#336,.T.);
#3949=EDGE_CURVE('',#3108,#3109,#886,.T.);
#3950=EDGE_CURVE('',#3108,#3106,#337,.T.);
#3951=EDGE_CURVE('',#3107,#3109,#338,.T.);
#3952=EDGE_CURVE('',#3110,#3111,#887,.T.);
#3953=EDGE_CURVE('',#3110,#3108,#339,.T.);
#3954=EDGE_CURVE('',#3109,#3111,#340,.T.);
#3955=EDGE_CURVE('',#3112,#3113,#888,.T.);
#3956=EDGE_CURVE('',#3112,#3110,#341,.T.);
#3957=EDGE_CURVE('',#3111,#3113,#342,.T.);
#3958=EDGE_CURVE('',#3114,#3115,#889,.T.);
#3959=EDGE_CURVE('',#3114,#3112,#343,.T.);
#3960=EDGE_CURVE('',#3113,#3115,#344,.T.);
#3961=EDGE_CURVE('',#3116,#3117,#890,.T.);
#3962=EDGE_CURVE('',#3116,#3114,#345,.T.);
#3963=EDGE_CURVE('',#3115,#3117,#346,.T.);
#3964=EDGE_CURVE('',#3118,#3118,#2604,.T.);
#3965=EDGE_CURVE('',#3118,#3119,#891,.T.);
#3966=EDGE_CURVE('',#3120,#3119,#347,.T.);
#3967=EDGE_CURVE('',#3121,#3120,#2605,.T.);
#3968=EDGE_CURVE('',#3105,#3121,#348,.T.);
#3969=EDGE_CURVE('',#3119,#3104,#349,.T.);
#3970=EDGE_CURVE('',#3122,#3116,#350,.T.);
#3971=EDGE_CURVE('',#3086,#3122,#351,.T.);
#3972=EDGE_CURVE('',#3120,#3100,#352,.T.);
#3973=EDGE_CURVE('',#3117,#3123,#353,.T.);
#3974=EDGE_CURVE('',#3122,#3123,#2606,.F.);
#3975=EDGE_CURVE('',#3124,#3125,#892,.T.);
#3976=EDGE_CURVE('',#3124,#3126,#893,.T.);
#3977=EDGE_CURVE('',#3126,#3127,#894,.T.);
#3978=EDGE_CURVE('',#3125,#3127,#895,.T.);
#3979=EDGE_CURVE('',#3128,#3124,#896,.T.);
#3980=EDGE_CURVE('',#3128,#3129,#897,.T.);
#3981=EDGE_CURVE('',#3129,#3126,#898,.T.);
#3982=EDGE_CURVE('',#3130,#3128,#899,.T.);
#3983=EDGE_CURVE('',#3130,#3131,#900,.T.);
#3984=EDGE_CURVE('',#3131,#3129,#901,.T.);
#3985=EDGE_CURVE('',#3132,#3130,#902,.T.);
#3986=EDGE_CURVE('',#3132,#3133,#903,.T.);
#3987=EDGE_CURVE('',#3133,#3131,#904,.T.);
#3988=EDGE_CURVE('',#3134,#3132,#905,.T.);
#3989=EDGE_CURVE('',#3134,#3135,#906,.T.);
#3990=EDGE_CURVE('',#3135,#3133,#907,.T.);
#3991=EDGE_CURVE('',#3125,#3134,#908,.T.);
#3992=EDGE_CURVE('',#3127,#3135,#909,.T.);
#3993=EDGE_CURVE('',#3121,#3101,#354,.T.);
#3994=EDGE_CURVE('',#3123,#3087,#355,.T.);
#3995=EDGE_CURVE('',#3136,#3136,#2607,.T.);
#3996=EDGE_CURVE('',#3137,#3137,#2608,.T.);
#3997=EDGE_CURVE('',#3138,#3138,#2609,.T.);
#3998=EDGE_CURVE('',#3138,#3136,#910,.T.);
#3999=EDGE_CURVE('',#3139,#3139,#2610,.T.);
#4000=EDGE_CURVE('',#3137,#3139,#911,.T.);
#4001=EDGE_CURVE('',#3140,#3141,#912,.T.);
#4002=EDGE_CURVE('',#3140,#3142,#356,.T.);
#4003=EDGE_CURVE('',#3142,#3143,#2611,.F.);
#4004=EDGE_CURVE('',#3143,#3141,#357,.T.);
#4005=EDGE_CURVE('',#3144,#3145,#913,.T.);
#4006=EDGE_CURVE('',#3144,#3140,#358,.T.);
#4007=EDGE_CURVE('',#3141,#3145,#359,.T.);
#4008=EDGE_CURVE('',#3146,#3147,#914,.T.);
#4009=EDGE_CURVE('',#3146,#3144,#360,.T.);
#4010=EDGE_CURVE('',#3145,#3147,#361,.T.);
#4011=EDGE_CURVE('',#3148,#3149,#915,.T.);
#4012=EDGE_CURVE('',#3148,#3146,#362,.T.);
#4013=EDGE_CURVE('',#3147,#3149,#363,.T.);
#4014=EDGE_CURVE('',#3150,#3151,#916,.T.);
#4015=EDGE_CURVE('',#3150,#3148,#364,.T.);
#4016=EDGE_CURVE('',#3149,#3151,#365,.T.);
#4017=EDGE_CURVE('',#3152,#3153,#917,.T.);
#4018=EDGE_CURVE('',#3152,#3150,#366,.T.);
#4019=EDGE_CURVE('',#3151,#3153,#367,.T.);
#4020=EDGE_CURVE('',#3154,#3155,#918,.T.);
#4021=EDGE_CURVE('',#3154,#3152,#368,.T.);
#4022=EDGE_CURVE('',#3153,#3155,#369,.T.);
#4023=EDGE_CURVE('',#3156,#3157,#919,.T.);
#4024=EDGE_CURVE('',#3156,#3154,#370,.T.);
#4025=EDGE_CURVE('',#3155,#3157,#371,.T.);
#4026=EDGE_CURVE('',#3158,#3159,#920,.T.);
#4027=EDGE_CURVE('',#3158,#3156,#372,.T.);
#4028=EDGE_CURVE('',#3157,#3159,#373,.T.);
#4029=EDGE_CURVE('',#3160,#3161,#921,.T.);
#4030=EDGE_CURVE('',#3160,#3158,#374,.T.);
#4031=EDGE_CURVE('',#3159,#3161,#375,.T.);
#4032=EDGE_CURVE('',#3162,#3163,#922,.T.);
#4033=EDGE_CURVE('',#3162,#3160,#376,.T.);
#4034=EDGE_CURVE('',#3161,#3163,#377,.T.);
#4035=EDGE_CURVE('',#3164,#3165,#923,.T.);
#4036=EDGE_CURVE('',#3164,#3162,#378,.T.);
#4037=EDGE_CURVE('',#3163,#3165,#379,.T.);
#4038=EDGE_CURVE('',#3166,#3167,#924,.T.);
#4039=EDGE_CURVE('',#3166,#3164,#380,.T.);
#4040=EDGE_CURVE('',#3165,#3167,#381,.T.);
#4041=EDGE_CURVE('',#3168,#3169,#925,.T.);
#4042=EDGE_CURVE('',#3168,#3170,#382,.T.);
#4043=EDGE_CURVE('',#3170,#3171,#2612,.T.);
#4044=EDGE_CURVE('',#3169,#3171,#383,.T.);
#4045=EDGE_CURVE('',#3172,#3173,#926,.T.);
#4046=EDGE_CURVE('',#3172,#3168,#384,.T.);
#4047=EDGE_CURVE('',#3173,#3169,#385,.T.);
#4048=EDGE_CURVE('',#3174,#3175,#927,.T.);
#4049=EDGE_CURVE('',#3174,#3172,#386,.T.);
#4050=EDGE_CURVE('',#3175,#3173,#387,.T.);
#4051=EDGE_CURVE('',#3176,#3177,#928,.T.);
#4052=EDGE_CURVE('',#3176,#3174,#388,.T.);
#4053=EDGE_CURVE('',#3177,#3175,#389,.T.);
#4054=EDGE_CURVE('',#3178,#3179,#929,.T.);
#4055=EDGE_CURVE('',#3178,#3176,#390,.T.);
#4056=EDGE_CURVE('',#3179,#3177,#391,.T.);
#4057=EDGE_CURVE('',#3180,#3181,#930,.T.);
#4058=EDGE_CURVE('',#3180,#3178,#392,.T.);
#4059=EDGE_CURVE('',#3181,#3179,#393,.T.);
#4060=EDGE_CURVE('',#3182,#3183,#931,.T.);
#4061=EDGE_CURVE('',#3182,#3180,#394,.T.);
#4062=EDGE_CURVE('',#3183,#3181,#395,.T.);
#4063=EDGE_CURVE('',#3184,#3185,#932,.T.);
#4064=EDGE_CURVE('',#3184,#3182,#396,.T.);
#4065=EDGE_CURVE('',#3185,#3183,#397,.T.);
#4066=EDGE_CURVE('',#3186,#3187,#933,.T.);
#4067=EDGE_CURVE('',#3186,#3184,#398,.T.);
#4068=EDGE_CURVE('',#3187,#3185,#399,.T.);
#4069=EDGE_CURVE('',#3188,#3189,#934,.T.);
#4070=EDGE_CURVE('',#3188,#3186,#400,.T.);
#4071=EDGE_CURVE('',#3189,#3187,#401,.T.);
#4072=EDGE_CURVE('',#3190,#3191,#935,.T.);
#4073=EDGE_CURVE('',#3190,#3188,#402,.T.);
#4074=EDGE_CURVE('',#3191,#3189,#403,.T.);
#4075=EDGE_CURVE('',#3192,#3193,#936,.T.);
#4076=EDGE_CURVE('',#3192,#3190,#404,.T.);
#4077=EDGE_CURVE('',#3193,#3191,#405,.T.);
#4078=EDGE_CURVE('',#3194,#3195,#937,.T.);
#4079=EDGE_CURVE('',#3194,#3192,#406,.T.);
#4080=EDGE_CURVE('',#3195,#3193,#407,.T.);
#4081=EDGE_CURVE('',#3171,#3196,#408,.T.);
#4082=EDGE_CURVE('',#3197,#3170,#409,.T.);
#4083=EDGE_CURVE('',#3198,#3197,#2613,.T.);
#4084=EDGE_CURVE('',#3196,#3198,#410,.T.);
#4085=EDGE_CURVE('',#3196,#3199,#938,.T.);
#4086=EDGE_CURVE('',#3199,#3199,#2614,.T.);
#4087=EDGE_CURVE('',#3200,#3194,#411,.T.);
#4088=EDGE_CURVE('',#3142,#3200,#412,.T.);
#4089=EDGE_CURVE('',#3197,#3166,#413,.T.);
#4090=EDGE_CURVE('',#3201,#3195,#414,.T.);
#4091=EDGE_CURVE('',#3200,#3201,#2615,.T.);
#4092=EDGE_CURVE('',#3167,#3198,#415,.T.);
#4093=EDGE_CURVE('',#3201,#3143,#416,.T.);
#4094=EDGE_CURVE('',#3202,#3203,#939,.T.);
#4095=EDGE_CURVE('',#3202,#3204,#940,.T.);
#4096=EDGE_CURVE('',#3204,#3205,#941,.T.);
#4097=EDGE_CURVE('',#3203,#3205,#942,.T.);
#4098=EDGE_CURVE('',#3206,#3202,#943,.T.);
#4099=EDGE_CURVE('',#3206,#3207,#944,.T.);
#4100=EDGE_CURVE('',#3207,#3204,#945,.T.);
#4101=EDGE_CURVE('',#3208,#3206,#946,.T.);
#4102=EDGE_CURVE('',#3208,#3209,#947,.T.);
#4103=EDGE_CURVE('',#3209,#3207,#948,.T.);
#4104=EDGE_CURVE('',#3210,#3208,#949,.T.);
#4105=EDGE_CURVE('',#3210,#3211,#950,.T.);
#4106=EDGE_CURVE('',#3211,#3209,#951,.T.);
#4107=EDGE_CURVE('',#3212,#3210,#952,.T.);
#4108=EDGE_CURVE('',#3212,#3213,#953,.T.);
#4109=EDGE_CURVE('',#3213,#3211,#954,.T.);
#4110=EDGE_CURVE('',#3203,#3212,#955,.T.);
#4111=EDGE_CURVE('',#3205,#3213,#956,.T.);
#4112=EDGE_CURVE('',#3214,#3214,#2616,.T.);
#4113=EDGE_CURVE('',#3214,#3215,#957,.T.);
#4114=EDGE_CURVE('',#3215,#3215,#2617,.T.);
#4115=ORIENTED_EDGE('',*,*,#3216,.F.);
#4116=ORIENTED_EDGE('',*,*,#3217,.T.);
#4117=ORIENTED_EDGE('',*,*,#3218,.F.);
#4118=ORIENTED_EDGE('',*,*,#3219,.T.);
#4119=ORIENTED_EDGE('',*,*,#3216,.T.);
#4120=ORIENTED_EDGE('',*,*,#3219,.F.);
#4121=ORIENTED_EDGE('',*,*,#3217,.F.);
#4122=ORIENTED_EDGE('',*,*,#3220,.T.);
#4123=ORIENTED_EDGE('',*,*,#3221,.F.);
#4124=ORIENTED_EDGE('',*,*,#3220,.F.);
#4125=ORIENTED_EDGE('',*,*,#3222,.F.);
#4126=ORIENTED_EDGE('',*,*,#3223,.T.);
#4127=ORIENTED_EDGE('',*,*,#3224,.F.);
#4128=ORIENTED_EDGE('',*,*,#3225,.T.);
#4129=ORIENTED_EDGE('',*,*,#3222,.T.);
#4130=ORIENTED_EDGE('',*,*,#3225,.F.);
#4131=ORIENTED_EDGE('',*,*,#3223,.F.);
#4132=ORIENTED_EDGE('',*,*,#3226,.T.);
#4133=ORIENTED_EDGE('',*,*,#3227,.F.);
#4134=ORIENTED_EDGE('',*,*,#3226,.F.);
#4135=ORIENTED_EDGE('',*,*,#3228,.F.);
#4136=ORIENTED_EDGE('',*,*,#3229,.T.);
#4137=ORIENTED_EDGE('',*,*,#3230,.F.);
#4138=ORIENTED_EDGE('',*,*,#3229,.F.);
#4139=ORIENTED_EDGE('',*,*,#3231,.F.);
#4140=ORIENTED_EDGE('',*,*,#3232,.T.);
#4141=ORIENTED_EDGE('',*,*,#3233,.F.);
#4142=ORIENTED_EDGE('',*,*,#3232,.F.);
#4143=ORIENTED_EDGE('',*,*,#3234,.F.);
#4144=ORIENTED_EDGE('',*,*,#3235,.T.);
#4145=ORIENTED_EDGE('',*,*,#3236,.F.);
#4146=ORIENTED_EDGE('',*,*,#3235,.F.);
#4147=ORIENTED_EDGE('',*,*,#3237,.F.);
#4148=ORIENTED_EDGE('',*,*,#3238,.T.);
#4149=ORIENTED_EDGE('',*,*,#3239,.F.);
#4150=ORIENTED_EDGE('',*,*,#3238,.F.);
#4151=ORIENTED_EDGE('',*,*,#3240,.F.);
#4152=ORIENTED_EDGE('',*,*,#3241,.T.);
#4153=ORIENTED_EDGE('',*,*,#3242,.F.);
#4154=ORIENTED_EDGE('',*,*,#3243,.F.);
#4155=ORIENTED_EDGE('',*,*,#3244,.F.);
#4156=ORIENTED_EDGE('',*,*,#3245,.T.);
#4157=ORIENTED_EDGE('',*,*,#3246,.F.);
#4158=ORIENTED_EDGE('',*,*,#3241,.F.);
#4159=ORIENTED_EDGE('',*,*,#3247,.F.);
#4160=ORIENTED_EDGE('',*,*,#3248,.T.);
#4161=ORIENTED_EDGE('',*,*,#3249,.F.);
#4162=ORIENTED_EDGE('',*,*,#3245,.F.);
#4163=ORIENTED_EDGE('',*,*,#3250,.F.);
#4164=ORIENTED_EDGE('',*,*,#3243,.T.);
#4165=ORIENTED_EDGE('',*,*,#3251,.F.);
#4166=ORIENTED_EDGE('',*,*,#3248,.F.);
#4167=ORIENTED_EDGE('',*,*,#3252,.F.);
#4168=ORIENTED_EDGE('',*,*,#3253,.T.);
#4169=ORIENTED_EDGE('',*,*,#3254,.F.);
#4170=ORIENTED_EDGE('',*,*,#3255,.F.);
#4171=ORIENTED_EDGE('',*,*,#3256,.F.);
#4172=ORIENTED_EDGE('',*,*,#3257,.T.);
#4173=ORIENTED_EDGE('',*,*,#3258,.F.);
#4174=ORIENTED_EDGE('',*,*,#3253,.F.);
#4175=ORIENTED_EDGE('',*,*,#3259,.F.);
#4176=ORIENTED_EDGE('',*,*,#3260,.T.);
#4177=ORIENTED_EDGE('',*,*,#3261,.F.);
#4178=ORIENTED_EDGE('',*,*,#3257,.F.);
#4179=ORIENTED_EDGE('',*,*,#3262,.F.);
#4180=ORIENTED_EDGE('',*,*,#3255,.T.);
#4181=ORIENTED_EDGE('',*,*,#3263,.F.);
#4182=ORIENTED_EDGE('',*,*,#3260,.F.);
#4183=ORIENTED_EDGE('',*,*,#3264,.F.);
#4184=ORIENTED_EDGE('',*,*,#3265,.T.);
#4185=ORIENTED_EDGE('',*,*,#3266,.F.);
#4186=ORIENTED_EDGE('',*,*,#3267,.F.);
#4187=ORIENTED_EDGE('',*,*,#3268,.F.);
#4188=ORIENTED_EDGE('',*,*,#3269,.T.);
#4189=ORIENTED_EDGE('',*,*,#3270,.F.);
#4190=ORIENTED_EDGE('',*,*,#3271,.F.);
#4191=ORIENTED_EDGE('',*,*,#3272,.T.);
#4192=ORIENTED_EDGE('',*,*,#3270,.T.);
#4193=ORIENTED_EDGE('',*,*,#3273,.T.);
#4194=ORIENTED_EDGE('',*,*,#3266,.T.);
#4195=ORIENTED_EDGE('',*,*,#3264,.T.);
#4196=ORIENTED_EDGE('',*,*,#3274,.T.);
#4197=ORIENTED_EDGE('',*,*,#3275,.T.);
#4198=ORIENTED_EDGE('',*,*,#3276,.T.);
#4199=ORIENTED_EDGE('',*,*,#3224,.T.);
#4200=ORIENTED_EDGE('',*,*,#3234,.T.);
#4201=ORIENTED_EDGE('',*,*,#3237,.T.);
#4202=ORIENTED_EDGE('',*,*,#3268,.T.);
#4203=ORIENTED_EDGE('',*,*,#3277,.T.);
#4204=ORIENTED_EDGE('',*,*,#3278,.T.);
#4205=ORIENTED_EDGE('',*,*,#3279,.T.);
#4206=ORIENTED_EDGE('',*,*,#3240,.T.);
#4207=ORIENTED_EDGE('',*,*,#3250,.T.);
#4208=ORIENTED_EDGE('',*,*,#3247,.T.);
#4209=ORIENTED_EDGE('',*,*,#3244,.T.);
#4210=ORIENTED_EDGE('',*,*,#3252,.T.);
#4211=ORIENTED_EDGE('',*,*,#3262,.T.);
#4212=ORIENTED_EDGE('',*,*,#3259,.T.);
#4213=ORIENTED_EDGE('',*,*,#3256,.T.);
#4214=ORIENTED_EDGE('',*,*,#3278,.F.);
#4215=ORIENTED_EDGE('',*,*,#3280,.T.);
#4216=ORIENTED_EDGE('',*,*,#3281,.F.);
#4217=ORIENTED_EDGE('',*,*,#3282,.F.);
#4218=ORIENTED_EDGE('',*,*,#3283,.F.);
#4219=ORIENTED_EDGE('',*,*,#3284,.T.);
#4220=ORIENTED_EDGE('',*,*,#3285,.F.);
#4221=ORIENTED_EDGE('',*,*,#3286,.F.);
#4222=ORIENTED_EDGE('',*,*,#3287,.T.);
#4223=ORIENTED_EDGE('',*,*,#3285,.T.);
#4224=ORIENTED_EDGE('',*,*,#3288,.T.);
#4225=ORIENTED_EDGE('',*,*,#3281,.T.);
#4226=ORIENTED_EDGE('',*,*,#3283,.T.);
#4227=ORIENTED_EDGE('',*,*,#3289,.T.);
#4228=ORIENTED_EDGE('',*,*,#3290,.T.);
#4229=ORIENTED_EDGE('',*,*,#3291,.T.);
#4230=ORIENTED_EDGE('',*,*,#3218,.T.);
#4231=ORIENTED_EDGE('',*,*,#3228,.T.);
#4232=ORIENTED_EDGE('',*,*,#3231,.T.);
#4233=ORIENTED_EDGE('',*,*,#3292,.T.);
#4234=ORIENTED_EDGE('',*,*,#3293,.T.);
#4235=ORIENTED_EDGE('',*,*,#3275,.F.);
#4236=ORIENTED_EDGE('',*,*,#3294,.F.);
#4237=ORIENTED_EDGE('',*,*,#3295,.T.);
#4238=ORIENTED_EDGE('',*,*,#3294,.T.);
#4239=ORIENTED_EDGE('',*,*,#3274,.F.);
#4240=ORIENTED_EDGE('',*,*,#3267,.T.);
#4241=ORIENTED_EDGE('',*,*,#3273,.F.);
#4242=ORIENTED_EDGE('',*,*,#3269,.F.);
#4243=ORIENTED_EDGE('',*,*,#3279,.F.);
#4244=ORIENTED_EDGE('',*,*,#3282,.T.);
#4245=ORIENTED_EDGE('',*,*,#3288,.F.);
#4246=ORIENTED_EDGE('',*,*,#3284,.F.);
#4247=ORIENTED_EDGE('',*,*,#3291,.F.);
#4248=ORIENTED_EDGE('',*,*,#3296,.F.);
#4249=ORIENTED_EDGE('',*,*,#3297,.T.);
#4250=ORIENTED_EDGE('',*,*,#3296,.T.);
#4251=ORIENTED_EDGE('',*,*,#3290,.F.);
#4252=ORIENTED_EDGE('',*,*,#3298,.F.);
#4253=ORIENTED_EDGE('',*,*,#3299,.T.);
#4254=ORIENTED_EDGE('',*,*,#3298,.T.);
#4255=ORIENTED_EDGE('',*,*,#3289,.F.);
#4256=ORIENTED_EDGE('',*,*,#3286,.T.);
#4257=ORIENTED_EDGE('',*,*,#3287,.F.);
#4258=ORIENTED_EDGE('',*,*,#3280,.F.);
#4259=ORIENTED_EDGE('',*,*,#3277,.F.);
#4260=ORIENTED_EDGE('',*,*,#3271,.T.);
#4261=ORIENTED_EDGE('',*,*,#3272,.F.);
#4262=ORIENTED_EDGE('',*,*,#3265,.F.);
#4263=ORIENTED_EDGE('',*,*,#3276,.F.);
#4264=ORIENTED_EDGE('',*,*,#3293,.F.);
#4265=ORIENTED_EDGE('',*,*,#3299,.F.);
#4266=ORIENTED_EDGE('',*,*,#3292,.F.);
#4267=ORIENTED_EDGE('',*,*,#3295,.F.);
#4268=ORIENTED_EDGE('',*,*,#3297,.F.);
#4269=ORIENTED_EDGE('',*,*,#3230,.T.);
#4270=ORIENTED_EDGE('',*,*,#3233,.T.);
#4271=ORIENTED_EDGE('',*,*,#3236,.T.);
#4272=ORIENTED_EDGE('',*,*,#3239,.T.);
#4273=ORIENTED_EDGE('',*,*,#3242,.T.);
#4274=ORIENTED_EDGE('',*,*,#3246,.T.);
#4275=ORIENTED_EDGE('',*,*,#3249,.T.);
#4276=ORIENTED_EDGE('',*,*,#3251,.T.);
#4277=ORIENTED_EDGE('',*,*,#3254,.T.);
#4278=ORIENTED_EDGE('',*,*,#3258,.T.);
#4279=ORIENTED_EDGE('',*,*,#3261,.T.);
#4280=ORIENTED_EDGE('',*,*,#3263,.T.);
#4281=ORIENTED_EDGE('',*,*,#3227,.T.);
#4282=ORIENTED_EDGE('',*,*,#3221,.T.);
#4283=ORIENTED_EDGE('',*,*,#3300,.T.);
#4284=ORIENTED_EDGE('',*,*,#3301,.T.);
#4285=ORIENTED_EDGE('',*,*,#3302,.T.);
#4286=ORIENTED_EDGE('',*,*,#3303,.T.);
#4287=ORIENTED_EDGE('',*,*,#3304,.T.);
#4288=ORIENTED_EDGE('',*,*,#3305,.T.);
#4289=ORIENTED_EDGE('',*,*,#3304,.F.);
#4290=ORIENTED_EDGE('',*,*,#3306,.T.);
#4291=ORIENTED_EDGE('',*,*,#3307,.T.);
#4292=ORIENTED_EDGE('',*,*,#3308,.T.);
#4293=ORIENTED_EDGE('',*,*,#3300,.F.);
#4294=ORIENTED_EDGE('',*,*,#3309,.T.);
#4295=ORIENTED_EDGE('',*,*,#3310,.T.);
#4296=ORIENTED_EDGE('',*,*,#3311,.T.);
#4297=ORIENTED_EDGE('',*,*,#3307,.F.);
#4298=ORIENTED_EDGE('',*,*,#3312,.T.);
#4299=ORIENTED_EDGE('',*,*,#3313,.T.);
#4300=ORIENTED_EDGE('',*,*,#3314,.T.);
#4301=ORIENTED_EDGE('',*,*,#3310,.F.);
#4302=ORIENTED_EDGE('',*,*,#3315,.T.);
#4303=ORIENTED_EDGE('',*,*,#3316,.T.);
#4304=ORIENTED_EDGE('',*,*,#3317,.T.);
#4305=ORIENTED_EDGE('',*,*,#3313,.F.);
#4306=ORIENTED_EDGE('',*,*,#3318,.T.);
#4307=ORIENTED_EDGE('',*,*,#3319,.T.);
#4308=ORIENTED_EDGE('',*,*,#3320,.T.);
#4309=ORIENTED_EDGE('',*,*,#3316,.F.);
#4310=ORIENTED_EDGE('',*,*,#3321,.T.);
#4311=ORIENTED_EDGE('',*,*,#3322,.T.);
#4312=ORIENTED_EDGE('',*,*,#3323,.T.);
#4313=ORIENTED_EDGE('',*,*,#3319,.F.);
#4314=ORIENTED_EDGE('',*,*,#3324,.T.);
#4315=ORIENTED_EDGE('',*,*,#3325,.T.);
#4316=ORIENTED_EDGE('',*,*,#3326,.T.);
#4317=ORIENTED_EDGE('',*,*,#3322,.F.);
#4318=ORIENTED_EDGE('',*,*,#3327,.T.);
#4319=ORIENTED_EDGE('',*,*,#3328,.T.);
#4320=ORIENTED_EDGE('',*,*,#3329,.T.);
#4321=ORIENTED_EDGE('',*,*,#3325,.F.);
#4322=ORIENTED_EDGE('',*,*,#3330,.T.);
#4323=ORIENTED_EDGE('',*,*,#3331,.T.);
#4324=ORIENTED_EDGE('',*,*,#3332,.T.);
#4325=ORIENTED_EDGE('',*,*,#3328,.F.);
#4326=ORIENTED_EDGE('',*,*,#3333,.T.);
#4327=ORIENTED_EDGE('',*,*,#3334,.T.);
#4328=ORIENTED_EDGE('',*,*,#3335,.T.);
#4329=ORIENTED_EDGE('',*,*,#3331,.F.);
#4330=ORIENTED_EDGE('',*,*,#3336,.T.);
#4331=ORIENTED_EDGE('',*,*,#3337,.T.);
#4332=ORIENTED_EDGE('',*,*,#3338,.T.);
#4333=ORIENTED_EDGE('',*,*,#3334,.F.);
#4334=ORIENTED_EDGE('',*,*,#3339,.T.);
#4335=ORIENTED_EDGE('',*,*,#3340,.T.);
#4336=ORIENTED_EDGE('',*,*,#3341,.T.);
#4337=ORIENTED_EDGE('',*,*,#3337,.F.);
#4338=ORIENTED_EDGE('',*,*,#3342,.T.);
#4339=ORIENTED_EDGE('',*,*,#3343,.T.);
#4340=ORIENTED_EDGE('',*,*,#3344,.T.);
#4341=ORIENTED_EDGE('',*,*,#3340,.F.);
#4342=ORIENTED_EDGE('',*,*,#3345,.T.);
#4343=ORIENTED_EDGE('',*,*,#3346,.F.);
#4344=ORIENTED_EDGE('',*,*,#3347,.T.);
#4345=ORIENTED_EDGE('',*,*,#3348,.F.);
#4346=ORIENTED_EDGE('',*,*,#3349,.T.);
#4347=ORIENTED_EDGE('',*,*,#3350,.T.);
#4348=ORIENTED_EDGE('',*,*,#3351,.T.);
#4349=ORIENTED_EDGE('',*,*,#3352,.F.);
#4350=ORIENTED_EDGE('',*,*,#3353,.F.);
#4351=ORIENTED_EDGE('',*,*,#3354,.T.);
#4352=ORIENTED_EDGE('',*,*,#3355,.T.);
#4353=ORIENTED_EDGE('',*,*,#3350,.F.);
#4354=ORIENTED_EDGE('',*,*,#3356,.F.);
#4355=ORIENTED_EDGE('',*,*,#3357,.T.);
#4356=ORIENTED_EDGE('',*,*,#3358,.T.);
#4357=ORIENTED_EDGE('',*,*,#3354,.F.);
#4358=ORIENTED_EDGE('',*,*,#3359,.F.);
#4359=ORIENTED_EDGE('',*,*,#3360,.T.);
#4360=ORIENTED_EDGE('',*,*,#3361,.T.);
#4361=ORIENTED_EDGE('',*,*,#3357,.F.);
#4362=ORIENTED_EDGE('',*,*,#3362,.F.);
#4363=ORIENTED_EDGE('',*,*,#3363,.T.);
#4364=ORIENTED_EDGE('',*,*,#3364,.T.);
#4365=ORIENTED_EDGE('',*,*,#3360,.F.);
#4366=ORIENTED_EDGE('',*,*,#3365,.F.);
#4367=ORIENTED_EDGE('',*,*,#3366,.T.);
#4368=ORIENTED_EDGE('',*,*,#3367,.T.);
#4369=ORIENTED_EDGE('',*,*,#3363,.F.);
#4370=ORIENTED_EDGE('',*,*,#3368,.F.);
#4371=ORIENTED_EDGE('',*,*,#3369,.T.);
#4372=ORIENTED_EDGE('',*,*,#3370,.T.);
#4373=ORIENTED_EDGE('',*,*,#3366,.F.);
#4374=ORIENTED_EDGE('',*,*,#3371,.F.);
#4375=ORIENTED_EDGE('',*,*,#3372,.T.);
#4376=ORIENTED_EDGE('',*,*,#3373,.T.);
#4377=ORIENTED_EDGE('',*,*,#3369,.F.);
#4378=ORIENTED_EDGE('',*,*,#3374,.F.);
#4379=ORIENTED_EDGE('',*,*,#3375,.T.);
#4380=ORIENTED_EDGE('',*,*,#3376,.T.);
#4381=ORIENTED_EDGE('',*,*,#3372,.F.);
#4382=ORIENTED_EDGE('',*,*,#3377,.F.);
#4383=ORIENTED_EDGE('',*,*,#3378,.T.);
#4384=ORIENTED_EDGE('',*,*,#3379,.T.);
#4385=ORIENTED_EDGE('',*,*,#3375,.F.);
#4386=ORIENTED_EDGE('',*,*,#3380,.F.);
#4387=ORIENTED_EDGE('',*,*,#3381,.T.);
#4388=ORIENTED_EDGE('',*,*,#3382,.T.);
#4389=ORIENTED_EDGE('',*,*,#3378,.F.);
#4390=ORIENTED_EDGE('',*,*,#3383,.F.);
#4391=ORIENTED_EDGE('',*,*,#3384,.T.);
#4392=ORIENTED_EDGE('',*,*,#3385,.T.);
#4393=ORIENTED_EDGE('',*,*,#3381,.F.);
#4394=ORIENTED_EDGE('',*,*,#3386,.F.);
#4395=ORIENTED_EDGE('',*,*,#3387,.T.);
#4396=ORIENTED_EDGE('',*,*,#3388,.T.);
#4397=ORIENTED_EDGE('',*,*,#3384,.F.);
#4398=ORIENTED_EDGE('',*,*,#3389,.F.);
#4399=ORIENTED_EDGE('',*,*,#3390,.T.);
#4400=ORIENTED_EDGE('',*,*,#3391,.T.);
#4401=ORIENTED_EDGE('',*,*,#3387,.F.);
#4402=ORIENTED_EDGE('',*,*,#3392,.F.);
#4403=ORIENTED_EDGE('',*,*,#3393,.T.);
#4404=ORIENTED_EDGE('',*,*,#3394,.T.);
#4405=ORIENTED_EDGE('',*,*,#3390,.F.);
#4406=ORIENTED_EDGE('',*,*,#3395,.F.);
#4407=ORIENTED_EDGE('',*,*,#3396,.F.);
#4408=ORIENTED_EDGE('',*,*,#3397,.F.);
#4409=ORIENTED_EDGE('',*,*,#3398,.F.);
#4410=ORIENTED_EDGE('',*,*,#3399,.T.);
#4411=ORIENTED_EDGE('',*,*,#3400,.T.);
#4412=ORIENTED_EDGE('',*,*,#3401,.T.);
#4413=ORIENTED_EDGE('',*,*,#3402,.T.);
#4414=ORIENTED_EDGE('',*,*,#3403,.T.);
#4415=ORIENTED_EDGE('',*,*,#3404,.T.);
#4416=ORIENTED_EDGE('',*,*,#3405,.T.);
#4417=ORIENTED_EDGE('',*,*,#3404,.F.);
#4418=ORIENTED_EDGE('',*,*,#3406,.T.);
#4419=ORIENTED_EDGE('',*,*,#3407,.T.);
#4420=ORIENTED_EDGE('',*,*,#3408,.T.);
#4421=ORIENTED_EDGE('',*,*,#3400,.F.);
#4422=ORIENTED_EDGE('',*,*,#3409,.T.);
#4423=ORIENTED_EDGE('',*,*,#3410,.T.);
#4424=ORIENTED_EDGE('',*,*,#3411,.T.);
#4425=ORIENTED_EDGE('',*,*,#3407,.F.);
#4426=ORIENTED_EDGE('',*,*,#3412,.T.);
#4427=ORIENTED_EDGE('',*,*,#3413,.T.);
#4428=ORIENTED_EDGE('',*,*,#3414,.T.);
#4429=ORIENTED_EDGE('',*,*,#3410,.F.);
#4430=ORIENTED_EDGE('',*,*,#3415,.T.);
#4431=ORIENTED_EDGE('',*,*,#3416,.T.);
#4432=ORIENTED_EDGE('',*,*,#3417,.T.);
#4433=ORIENTED_EDGE('',*,*,#3413,.F.);
#4434=ORIENTED_EDGE('',*,*,#3418,.T.);
#4435=ORIENTED_EDGE('',*,*,#3419,.T.);
#4436=ORIENTED_EDGE('',*,*,#3420,.T.);
#4437=ORIENTED_EDGE('',*,*,#3416,.F.);
#4438=ORIENTED_EDGE('',*,*,#3421,.T.);
#4439=ORIENTED_EDGE('',*,*,#3422,.T.);
#4440=ORIENTED_EDGE('',*,*,#3423,.T.);
#4441=ORIENTED_EDGE('',*,*,#3419,.F.);
#4442=ORIENTED_EDGE('',*,*,#3424,.T.);
#4443=ORIENTED_EDGE('',*,*,#3425,.T.);
#4444=ORIENTED_EDGE('',*,*,#3426,.T.);
#4445=ORIENTED_EDGE('',*,*,#3422,.F.);
#4446=ORIENTED_EDGE('',*,*,#3427,.T.);
#4447=ORIENTED_EDGE('',*,*,#3428,.T.);
#4448=ORIENTED_EDGE('',*,*,#3429,.T.);
#4449=ORIENTED_EDGE('',*,*,#3425,.F.);
#4450=ORIENTED_EDGE('',*,*,#3430,.T.);
#4451=ORIENTED_EDGE('',*,*,#3431,.T.);
#4452=ORIENTED_EDGE('',*,*,#3432,.T.);
#4453=ORIENTED_EDGE('',*,*,#3428,.F.);
#4454=ORIENTED_EDGE('',*,*,#3433,.T.);
#4455=ORIENTED_EDGE('',*,*,#3434,.T.);
#4456=ORIENTED_EDGE('',*,*,#3435,.T.);
#4457=ORIENTED_EDGE('',*,*,#3431,.F.);
#4458=ORIENTED_EDGE('',*,*,#3436,.T.);
#4459=ORIENTED_EDGE('',*,*,#3437,.T.);
#4460=ORIENTED_EDGE('',*,*,#3438,.T.);
#4461=ORIENTED_EDGE('',*,*,#3434,.F.);
#4462=ORIENTED_EDGE('',*,*,#3439,.T.);
#4463=ORIENTED_EDGE('',*,*,#3440,.T.);
#4464=ORIENTED_EDGE('',*,*,#3441,.T.);
#4465=ORIENTED_EDGE('',*,*,#3437,.F.);
#4466=ORIENTED_EDGE('',*,*,#3442,.T.);
#4467=ORIENTED_EDGE('',*,*,#3443,.T.);
#4468=ORIENTED_EDGE('',*,*,#3444,.T.);
#4469=ORIENTED_EDGE('',*,*,#3440,.F.);
#4470=ORIENTED_EDGE('',*,*,#3445,.T.);
#4471=ORIENTED_EDGE('',*,*,#3446,.F.);
#4472=ORIENTED_EDGE('',*,*,#3447,.T.);
#4473=ORIENTED_EDGE('',*,*,#3448,.F.);
#4474=ORIENTED_EDGE('',*,*,#3449,.T.);
#4475=ORIENTED_EDGE('',*,*,#3450,.T.);
#4476=ORIENTED_EDGE('',*,*,#3451,.T.);
#4477=ORIENTED_EDGE('',*,*,#3452,.F.);
#4478=ORIENTED_EDGE('',*,*,#3453,.F.);
#4479=ORIENTED_EDGE('',*,*,#3454,.T.);
#4480=ORIENTED_EDGE('',*,*,#3455,.T.);
#4481=ORIENTED_EDGE('',*,*,#3450,.F.);
#4482=ORIENTED_EDGE('',*,*,#3456,.F.);
#4483=ORIENTED_EDGE('',*,*,#3457,.T.);
#4484=ORIENTED_EDGE('',*,*,#3458,.T.);
#4485=ORIENTED_EDGE('',*,*,#3454,.F.);
#4486=ORIENTED_EDGE('',*,*,#3459,.F.);
#4487=ORIENTED_EDGE('',*,*,#3460,.T.);
#4488=ORIENTED_EDGE('',*,*,#3461,.T.);
#4489=ORIENTED_EDGE('',*,*,#3457,.F.);
#4490=ORIENTED_EDGE('',*,*,#3462,.F.);
#4491=ORIENTED_EDGE('',*,*,#3463,.T.);
#4492=ORIENTED_EDGE('',*,*,#3464,.T.);
#4493=ORIENTED_EDGE('',*,*,#3460,.F.);
#4494=ORIENTED_EDGE('',*,*,#3465,.F.);
#4495=ORIENTED_EDGE('',*,*,#3466,.T.);
#4496=ORIENTED_EDGE('',*,*,#3467,.T.);
#4497=ORIENTED_EDGE('',*,*,#3463,.F.);
#4498=ORIENTED_EDGE('',*,*,#3468,.F.);
#4499=ORIENTED_EDGE('',*,*,#3469,.T.);
#4500=ORIENTED_EDGE('',*,*,#3470,.T.);
#4501=ORIENTED_EDGE('',*,*,#3466,.F.);
#4502=ORIENTED_EDGE('',*,*,#3471,.F.);
#4503=ORIENTED_EDGE('',*,*,#3472,.T.);
#4504=ORIENTED_EDGE('',*,*,#3473,.T.);
#4505=ORIENTED_EDGE('',*,*,#3469,.F.);
#4506=ORIENTED_EDGE('',*,*,#3474,.F.);
#4507=ORIENTED_EDGE('',*,*,#3475,.T.);
#4508=ORIENTED_EDGE('',*,*,#3476,.T.);
#4509=ORIENTED_EDGE('',*,*,#3472,.F.);
#4510=ORIENTED_EDGE('',*,*,#3477,.F.);
#4511=ORIENTED_EDGE('',*,*,#3478,.T.);
#4512=ORIENTED_EDGE('',*,*,#3479,.T.);
#4513=ORIENTED_EDGE('',*,*,#3475,.F.);
#4514=ORIENTED_EDGE('',*,*,#3480,.F.);
#4515=ORIENTED_EDGE('',*,*,#3481,.T.);
#4516=ORIENTED_EDGE('',*,*,#3482,.T.);
#4517=ORIENTED_EDGE('',*,*,#3478,.F.);
#4518=ORIENTED_EDGE('',*,*,#3483,.F.);
#4519=ORIENTED_EDGE('',*,*,#3484,.T.);
#4520=ORIENTED_EDGE('',*,*,#3485,.T.);
#4521=ORIENTED_EDGE('',*,*,#3481,.F.);
#4522=ORIENTED_EDGE('',*,*,#3486,.F.);
#4523=ORIENTED_EDGE('',*,*,#3487,.T.);
#4524=ORIENTED_EDGE('',*,*,#3488,.T.);
#4525=ORIENTED_EDGE('',*,*,#3484,.F.);
#4526=ORIENTED_EDGE('',*,*,#3489,.F.);
#4527=ORIENTED_EDGE('',*,*,#3490,.T.);
#4528=ORIENTED_EDGE('',*,*,#3491,.T.);
#4529=ORIENTED_EDGE('',*,*,#3487,.F.);
#4530=ORIENTED_EDGE('',*,*,#3492,.F.);
#4531=ORIENTED_EDGE('',*,*,#3493,.T.);
#4532=ORIENTED_EDGE('',*,*,#3494,.T.);
#4533=ORIENTED_EDGE('',*,*,#3490,.F.);
#4534=ORIENTED_EDGE('',*,*,#3495,.F.);
#4535=ORIENTED_EDGE('',*,*,#3496,.F.);
#4536=ORIENTED_EDGE('',*,*,#3497,.F.);
#4537=ORIENTED_EDGE('',*,*,#3498,.F.);
#4538=ORIENTED_EDGE('',*,*,#3499,.T.);
#4539=ORIENTED_EDGE('',*,*,#3402,.F.);
#4540=ORIENTED_EDGE('',*,*,#3500,.T.);
#4541=ORIENTED_EDGE('',*,*,#3452,.T.);
#4542=ORIENTED_EDGE('',*,*,#3501,.T.);
#4543=ORIENTED_EDGE('',*,*,#3496,.T.);
#4544=ORIENTED_EDGE('',*,*,#3502,.T.);
#4545=ORIENTED_EDGE('',*,*,#3493,.F.);
#4546=ORIENTED_EDGE('',*,*,#3503,.F.);
#4547=ORIENTED_EDGE('',*,*,#3501,.F.);
#4548=ORIENTED_EDGE('',*,*,#3451,.F.);
#4549=ORIENTED_EDGE('',*,*,#3455,.F.);
#4550=ORIENTED_EDGE('',*,*,#3458,.F.);
#4551=ORIENTED_EDGE('',*,*,#3461,.F.);
#4552=ORIENTED_EDGE('',*,*,#3464,.F.);
#4553=ORIENTED_EDGE('',*,*,#3467,.F.);
#4554=ORIENTED_EDGE('',*,*,#3470,.F.);
#4555=ORIENTED_EDGE('',*,*,#3473,.F.);
#4556=ORIENTED_EDGE('',*,*,#3476,.F.);
#4557=ORIENTED_EDGE('',*,*,#3479,.F.);
#4558=ORIENTED_EDGE('',*,*,#3482,.F.);
#4559=ORIENTED_EDGE('',*,*,#3485,.F.);
#4560=ORIENTED_EDGE('',*,*,#3488,.F.);
#4561=ORIENTED_EDGE('',*,*,#3491,.F.);
#4562=ORIENTED_EDGE('',*,*,#3494,.F.);
#4563=ORIENTED_EDGE('',*,*,#3502,.F.);
#4564=ORIENTED_EDGE('',*,*,#3499,.F.);
#4565=ORIENTED_EDGE('',*,*,#3504,.F.);
#4566=ORIENTED_EDGE('',*,*,#3447,.F.);
#4567=ORIENTED_EDGE('',*,*,#3505,.F.);
#4568=ORIENTED_EDGE('',*,*,#3445,.F.);
#4569=ORIENTED_EDGE('',*,*,#3442,.F.);
#4570=ORIENTED_EDGE('',*,*,#3439,.F.);
#4571=ORIENTED_EDGE('',*,*,#3436,.F.);
#4572=ORIENTED_EDGE('',*,*,#3433,.F.);
#4573=ORIENTED_EDGE('',*,*,#3430,.F.);
#4574=ORIENTED_EDGE('',*,*,#3427,.F.);
#4575=ORIENTED_EDGE('',*,*,#3424,.F.);
#4576=ORIENTED_EDGE('',*,*,#3421,.F.);
#4577=ORIENTED_EDGE('',*,*,#3418,.F.);
#4578=ORIENTED_EDGE('',*,*,#3415,.F.);
#4579=ORIENTED_EDGE('',*,*,#3412,.F.);
#4580=ORIENTED_EDGE('',*,*,#3409,.F.);
#4581=ORIENTED_EDGE('',*,*,#3406,.F.);
#4582=ORIENTED_EDGE('',*,*,#3403,.F.);
#4583=ORIENTED_EDGE('',*,*,#3500,.F.);
#4584=ORIENTED_EDGE('',*,*,#3401,.F.);
#4585=ORIENTED_EDGE('',*,*,#3408,.F.);
#4586=ORIENTED_EDGE('',*,*,#3411,.F.);
#4587=ORIENTED_EDGE('',*,*,#3414,.F.);
#4588=ORIENTED_EDGE('',*,*,#3417,.F.);
#4589=ORIENTED_EDGE('',*,*,#3420,.F.);
#4590=ORIENTED_EDGE('',*,*,#3423,.F.);
#4591=ORIENTED_EDGE('',*,*,#3426,.F.);
#4592=ORIENTED_EDGE('',*,*,#3429,.F.);
#4593=ORIENTED_EDGE('',*,*,#3432,.F.);
#4594=ORIENTED_EDGE('',*,*,#3435,.F.);
#4595=ORIENTED_EDGE('',*,*,#3438,.F.);
#4596=ORIENTED_EDGE('',*,*,#3441,.F.);
#4597=ORIENTED_EDGE('',*,*,#3444,.F.);
#4598=ORIENTED_EDGE('',*,*,#3506,.F.);
#4599=ORIENTED_EDGE('',*,*,#3449,.F.);
#4600=ORIENTED_EDGE('',*,*,#3507,.F.);
#4601=ORIENTED_EDGE('',*,*,#3497,.T.);
#4602=ORIENTED_EDGE('',*,*,#3503,.T.);
#4603=ORIENTED_EDGE('',*,*,#3495,.T.);
#4604=ORIENTED_EDGE('',*,*,#3492,.T.);
#4605=ORIENTED_EDGE('',*,*,#3489,.T.);
#4606=ORIENTED_EDGE('',*,*,#3486,.T.);
#4607=ORIENTED_EDGE('',*,*,#3483,.T.);
#4608=ORIENTED_EDGE('',*,*,#3480,.T.);
#4609=ORIENTED_EDGE('',*,*,#3477,.T.);
#4610=ORIENTED_EDGE('',*,*,#3474,.T.);
#4611=ORIENTED_EDGE('',*,*,#3471,.T.);
#4612=ORIENTED_EDGE('',*,*,#3468,.T.);
#4613=ORIENTED_EDGE('',*,*,#3465,.T.);
#4614=ORIENTED_EDGE('',*,*,#3462,.T.);
#4615=ORIENTED_EDGE('',*,*,#3459,.T.);
#4616=ORIENTED_EDGE('',*,*,#3456,.T.);
#4617=ORIENTED_EDGE('',*,*,#3453,.T.);
#4618=ORIENTED_EDGE('',*,*,#3446,.T.);
#4619=ORIENTED_EDGE('',*,*,#3506,.T.);
#4620=ORIENTED_EDGE('',*,*,#3443,.F.);
#4621=ORIENTED_EDGE('',*,*,#3505,.T.);
#4622=ORIENTED_EDGE('',*,*,#3302,.F.);
#4623=ORIENTED_EDGE('',*,*,#3508,.T.);
#4624=ORIENTED_EDGE('',*,*,#3352,.T.);
#4625=ORIENTED_EDGE('',*,*,#3509,.T.);
#4626=ORIENTED_EDGE('',*,*,#3396,.T.);
#4627=ORIENTED_EDGE('',*,*,#3510,.T.);
#4628=ORIENTED_EDGE('',*,*,#3393,.F.);
#4629=ORIENTED_EDGE('',*,*,#3511,.F.);
#4630=ORIENTED_EDGE('',*,*,#3509,.F.);
#4631=ORIENTED_EDGE('',*,*,#3351,.F.);
#4632=ORIENTED_EDGE('',*,*,#3355,.F.);
#4633=ORIENTED_EDGE('',*,*,#3358,.F.);
#4634=ORIENTED_EDGE('',*,*,#3361,.F.);
#4635=ORIENTED_EDGE('',*,*,#3364,.F.);
#4636=ORIENTED_EDGE('',*,*,#3367,.F.);
#4637=ORIENTED_EDGE('',*,*,#3370,.F.);
#4638=ORIENTED_EDGE('',*,*,#3373,.F.);
#4639=ORIENTED_EDGE('',*,*,#3376,.F.);
#4640=ORIENTED_EDGE('',*,*,#3379,.F.);
#4641=ORIENTED_EDGE('',*,*,#3382,.F.);
#4642=ORIENTED_EDGE('',*,*,#3385,.F.);
#4643=ORIENTED_EDGE('',*,*,#3388,.F.);
#4644=ORIENTED_EDGE('',*,*,#3391,.F.);
#4645=ORIENTED_EDGE('',*,*,#3394,.F.);
#4646=ORIENTED_EDGE('',*,*,#3510,.F.);
#4647=ORIENTED_EDGE('',*,*,#3399,.F.);
#4648=ORIENTED_EDGE('',*,*,#3512,.F.);
#4649=ORIENTED_EDGE('',*,*,#3347,.F.);
#4650=ORIENTED_EDGE('',*,*,#3513,.F.);
#4651=ORIENTED_EDGE('',*,*,#3345,.F.);
#4652=ORIENTED_EDGE('',*,*,#3342,.F.);
#4653=ORIENTED_EDGE('',*,*,#3339,.F.);
#4654=ORIENTED_EDGE('',*,*,#3336,.F.);
#4655=ORIENTED_EDGE('',*,*,#3333,.F.);
#4656=ORIENTED_EDGE('',*,*,#3330,.F.);
#4657=ORIENTED_EDGE('',*,*,#3327,.F.);
#4658=ORIENTED_EDGE('',*,*,#3324,.F.);
#4659=ORIENTED_EDGE('',*,*,#3321,.F.);
#4660=ORIENTED_EDGE('',*,*,#3318,.F.);
#4661=ORIENTED_EDGE('',*,*,#3315,.F.);
#4662=ORIENTED_EDGE('',*,*,#3312,.F.);
#4663=ORIENTED_EDGE('',*,*,#3309,.F.);
#4664=ORIENTED_EDGE('',*,*,#3306,.F.);
#4665=ORIENTED_EDGE('',*,*,#3303,.F.);
#4666=ORIENTED_EDGE('',*,*,#3508,.F.);
#4667=ORIENTED_EDGE('',*,*,#3301,.F.);
#4668=ORIENTED_EDGE('',*,*,#3308,.F.);
#4669=ORIENTED_EDGE('',*,*,#3311,.F.);
#4670=ORIENTED_EDGE('',*,*,#3314,.F.);
#4671=ORIENTED_EDGE('',*,*,#3317,.F.);
#4672=ORIENTED_EDGE('',*,*,#3320,.F.);
#4673=ORIENTED_EDGE('',*,*,#3323,.F.);
#4674=ORIENTED_EDGE('',*,*,#3326,.F.);
#4675=ORIENTED_EDGE('',*,*,#3329,.F.);
#4676=ORIENTED_EDGE('',*,*,#3332,.F.);
#4677=ORIENTED_EDGE('',*,*,#3335,.F.);
#4678=ORIENTED_EDGE('',*,*,#3338,.F.);
#4679=ORIENTED_EDGE('',*,*,#3341,.F.);
#4680=ORIENTED_EDGE('',*,*,#3344,.F.);
#4681=ORIENTED_EDGE('',*,*,#3514,.F.);
#4682=ORIENTED_EDGE('',*,*,#3349,.F.);
#4683=ORIENTED_EDGE('',*,*,#3515,.F.);
#4684=ORIENTED_EDGE('',*,*,#3397,.T.);
#4685=ORIENTED_EDGE('',*,*,#3511,.T.);
#4686=ORIENTED_EDGE('',*,*,#3395,.T.);
#4687=ORIENTED_EDGE('',*,*,#3392,.T.);
#4688=ORIENTED_EDGE('',*,*,#3389,.T.);
#4689=ORIENTED_EDGE('',*,*,#3386,.T.);
#4690=ORIENTED_EDGE('',*,*,#3383,.T.);
#4691=ORIENTED_EDGE('',*,*,#3380,.T.);
#4692=ORIENTED_EDGE('',*,*,#3377,.T.);
#4693=ORIENTED_EDGE('',*,*,#3374,.T.);
#4694=ORIENTED_EDGE('',*,*,#3371,.T.);
#4695=ORIENTED_EDGE('',*,*,#3368,.T.);
#4696=ORIENTED_EDGE('',*,*,#3365,.T.);
#4697=ORIENTED_EDGE('',*,*,#3362,.T.);
#4698=ORIENTED_EDGE('',*,*,#3359,.T.);
#4699=ORIENTED_EDGE('',*,*,#3356,.T.);
#4700=ORIENTED_EDGE('',*,*,#3353,.T.);
#4701=ORIENTED_EDGE('',*,*,#3346,.T.);
#4702=ORIENTED_EDGE('',*,*,#3514,.T.);
#4703=ORIENTED_EDGE('',*,*,#3343,.F.);
#4704=ORIENTED_EDGE('',*,*,#3513,.T.);
#4705=ORIENTED_EDGE('',*,*,#3405,.F.);
#4706=ORIENTED_EDGE('',*,*,#3305,.F.);
#4707=ORIENTED_EDGE('',*,*,#3516,.F.);
#4708=ORIENTED_EDGE('',*,*,#3517,.T.);
#4709=ORIENTED_EDGE('',*,*,#3518,.F.);
#4710=ORIENTED_EDGE('',*,*,#3517,.F.);
#4711=ORIENTED_EDGE('',*,*,#3519,.F.);
#4712=ORIENTED_EDGE('',*,*,#3520,.T.);
#4713=ORIENTED_EDGE('',*,*,#3521,.F.);
#4714=ORIENTED_EDGE('',*,*,#3520,.F.);
#4715=ORIENTED_EDGE('',*,*,#3522,.F.);
#4716=ORIENTED_EDGE('',*,*,#3523,.T.);
#4717=ORIENTED_EDGE('',*,*,#3524,.F.);
#4718=ORIENTED_EDGE('',*,*,#3523,.F.);
#4719=ORIENTED_EDGE('',*,*,#3525,.F.);
#4720=ORIENTED_EDGE('',*,*,#3526,.F.);
#4721=ORIENTED_EDGE('',*,*,#3527,.T.);
#4722=ORIENTED_EDGE('',*,*,#3528,.T.);
#4723=ORIENTED_EDGE('',*,*,#3529,.F.);
#4724=ORIENTED_EDGE('',*,*,#3530,.F.);
#4725=ORIENTED_EDGE('',*,*,#3531,.T.);
#4726=ORIENTED_EDGE('',*,*,#3532,.T.);
#4727=ORIENTED_EDGE('',*,*,#3527,.F.);
#4728=ORIENTED_EDGE('',*,*,#3533,.F.);
#4729=ORIENTED_EDGE('',*,*,#3531,.F.);
#4730=ORIENTED_EDGE('',*,*,#3534,.F.);
#4731=ORIENTED_EDGE('',*,*,#3525,.T.);
#4732=ORIENTED_EDGE('',*,*,#3535,.F.);
#4733=ORIENTED_EDGE('',*,*,#3536,.F.);
#4734=ORIENTED_EDGE('',*,*,#3537,.F.);
#4735=ORIENTED_EDGE('',*,*,#3529,.T.);
#4736=ORIENTED_EDGE('',*,*,#3538,.F.);
#4737=ORIENTED_EDGE('',*,*,#3539,.F.);
#4738=ORIENTED_EDGE('',*,*,#3540,.F.);
#4739=ORIENTED_EDGE('',*,*,#3541,.F.);
#4740=ORIENTED_EDGE('',*,*,#3542,.F.);
#4741=ORIENTED_EDGE('',*,*,#3543,.T.);
#4742=ORIENTED_EDGE('',*,*,#3544,.T.);
#4743=ORIENTED_EDGE('',*,*,#3524,.T.);
#4744=ORIENTED_EDGE('',*,*,#3545,.F.);
#4745=ORIENTED_EDGE('',*,*,#3546,.F.);
#4746=ORIENTED_EDGE('',*,*,#3547,.T.);
#4747=ORIENTED_EDGE('',*,*,#3542,.T.);
#4748=ORIENTED_EDGE('',*,*,#3548,.F.);
#4749=ORIENTED_EDGE('',*,*,#3544,.F.);
#4750=ORIENTED_EDGE('',*,*,#3549,.T.);
#4751=ORIENTED_EDGE('',*,*,#3550,.T.);
#4752=ORIENTED_EDGE('',*,*,#3547,.F.);
#4753=ORIENTED_EDGE('',*,*,#3551,.F.);
#4754=ORIENTED_EDGE('',*,*,#3549,.F.);
#4755=ORIENTED_EDGE('',*,*,#3543,.F.);
#4756=ORIENTED_EDGE('',*,*,#3545,.T.);
#4757=ORIENTED_EDGE('',*,*,#3541,.T.);
#4758=ORIENTED_EDGE('',*,*,#3548,.T.);
#4759=ORIENTED_EDGE('',*,*,#3552,.F.);
#4760=ORIENTED_EDGE('',*,*,#3553,.F.);
#4761=ORIENTED_EDGE('',*,*,#3554,.F.);
#4762=ORIENTED_EDGE('',*,*,#3555,.T.);
#4763=ORIENTED_EDGE('',*,*,#3556,.T.);
#4764=ORIENTED_EDGE('',*,*,#3557,.T.);
#4765=ORIENTED_EDGE('',*,*,#3558,.F.);
#4766=ORIENTED_EDGE('',*,*,#3559,.F.);
#4767=ORIENTED_EDGE('',*,*,#3560,.F.);
#4768=ORIENTED_EDGE('',*,*,#3561,.T.);
#4769=ORIENTED_EDGE('',*,*,#3562,.T.);
#4770=ORIENTED_EDGE('',*,*,#3563,.T.);
#4771=ORIENTED_EDGE('',*,*,#3564,.T.);
#4772=ORIENTED_EDGE('',*,*,#3565,.T.);
#4773=ORIENTED_EDGE('',*,*,#3566,.T.);
#4774=ORIENTED_EDGE('',*,*,#3567,.T.);
#4775=ORIENTED_EDGE('',*,*,#3568,.T.);
#4776=ORIENTED_EDGE('',*,*,#3537,.T.);
#4777=ORIENTED_EDGE('',*,*,#3569,.T.);
#4778=ORIENTED_EDGE('',*,*,#3556,.F.);
#4779=ORIENTED_EDGE('',*,*,#3570,.F.);
#4780=ORIENTED_EDGE('',*,*,#3538,.T.);
#4781=ORIENTED_EDGE('',*,*,#3532,.F.);
#4782=ORIENTED_EDGE('',*,*,#3533,.T.);
#4783=ORIENTED_EDGE('',*,*,#3526,.T.);
#4784=ORIENTED_EDGE('',*,*,#3516,.T.);
#4785=ORIENTED_EDGE('',*,*,#3519,.T.);
#4786=ORIENTED_EDGE('',*,*,#3555,.F.);
#4787=ORIENTED_EDGE('',*,*,#3571,.F.);
#4788=ORIENTED_EDGE('',*,*,#3539,.T.);
#4789=ORIENTED_EDGE('',*,*,#3570,.T.);
#4790=ORIENTED_EDGE('',*,*,#3557,.F.);
#4791=ORIENTED_EDGE('',*,*,#3569,.F.);
#4792=ORIENTED_EDGE('',*,*,#3536,.T.);
#4793=ORIENTED_EDGE('',*,*,#3572,.T.);
#4794=ORIENTED_EDGE('',*,*,#3540,.T.);
#4795=ORIENTED_EDGE('',*,*,#3571,.T.);
#4796=ORIENTED_EDGE('',*,*,#3554,.T.);
#4797=ORIENTED_EDGE('',*,*,#3573,.T.);
#4798=ORIENTED_EDGE('',*,*,#3574,.F.);
#4799=ORIENTED_EDGE('',*,*,#3575,.T.);
#4800=ORIENTED_EDGE('',*,*,#3576,.T.);
#4801=ORIENTED_EDGE('',*,*,#3577,.T.);
#4802=ORIENTED_EDGE('',*,*,#3578,.F.);
#4803=ORIENTED_EDGE('',*,*,#3579,.F.);
#4804=ORIENTED_EDGE('',*,*,#3558,.T.);
#4805=ORIENTED_EDGE('',*,*,#3572,.F.);
#4806=ORIENTED_EDGE('',*,*,#3535,.T.);
#4807=ORIENTED_EDGE('',*,*,#3528,.F.);
#4808=ORIENTED_EDGE('',*,*,#3534,.T.);
#4809=ORIENTED_EDGE('',*,*,#3530,.T.);
#4810=ORIENTED_EDGE('',*,*,#3518,.T.);
#4811=ORIENTED_EDGE('',*,*,#3521,.T.);
#4812=ORIENTED_EDGE('',*,*,#3580,.F.);
#4813=ORIENTED_EDGE('',*,*,#3581,.T.);
#4814=ORIENTED_EDGE('',*,*,#3565,.F.);
#4815=ORIENTED_EDGE('',*,*,#3582,.F.);
#4816=ORIENTED_EDGE('',*,*,#3583,.F.);
#4817=ORIENTED_EDGE('',*,*,#3584,.T.);
#4818=ORIENTED_EDGE('',*,*,#3566,.F.);
#4819=ORIENTED_EDGE('',*,*,#3581,.F.);
#4820=ORIENTED_EDGE('',*,*,#3585,.F.);
#4821=ORIENTED_EDGE('',*,*,#3586,.T.);
#4822=ORIENTED_EDGE('',*,*,#3567,.F.);
#4823=ORIENTED_EDGE('',*,*,#3584,.F.);
#4824=ORIENTED_EDGE('',*,*,#3587,.F.);
#4825=ORIENTED_EDGE('',*,*,#3582,.T.);
#4826=ORIENTED_EDGE('',*,*,#3568,.F.);
#4827=ORIENTED_EDGE('',*,*,#3586,.F.);
#4828=ORIENTED_EDGE('',*,*,#3588,.F.);
#4829=ORIENTED_EDGE('',*,*,#3589,.T.);
#4830=ORIENTED_EDGE('',*,*,#3561,.F.);
#4831=ORIENTED_EDGE('',*,*,#3590,.F.);
#4832=ORIENTED_EDGE('',*,*,#3591,.F.);
#4833=ORIENTED_EDGE('',*,*,#3592,.T.);
#4834=ORIENTED_EDGE('',*,*,#3562,.F.);
#4835=ORIENTED_EDGE('',*,*,#3589,.F.);
#4836=ORIENTED_EDGE('',*,*,#3593,.F.);
#4837=ORIENTED_EDGE('',*,*,#3594,.T.);
#4838=ORIENTED_EDGE('',*,*,#3563,.F.);
#4839=ORIENTED_EDGE('',*,*,#3592,.F.);
#4840=ORIENTED_EDGE('',*,*,#3595,.F.);
#4841=ORIENTED_EDGE('',*,*,#3590,.T.);
#4842=ORIENTED_EDGE('',*,*,#3564,.F.);
#4843=ORIENTED_EDGE('',*,*,#3594,.F.);
#4844=ORIENTED_EDGE('',*,*,#3596,.F.);
#4845=ORIENTED_EDGE('',*,*,#3597,.F.);
#4846=ORIENTED_EDGE('',*,*,#3577,.F.);
#4847=ORIENTED_EDGE('',*,*,#3598,.T.);
#4848=ORIENTED_EDGE('',*,*,#3599,.T.);
#4849=ORIENTED_EDGE('',*,*,#3600,.F.);
#4850=ORIENTED_EDGE('',*,*,#3601,.F.);
#4851=ORIENTED_EDGE('',*,*,#3602,.T.);
#4852=ORIENTED_EDGE('',*,*,#3576,.F.);
#4853=ORIENTED_EDGE('',*,*,#3603,.F.);
#4854=ORIENTED_EDGE('',*,*,#3604,.F.);
#4855=ORIENTED_EDGE('',*,*,#3598,.F.);
#4856=ORIENTED_EDGE('',*,*,#3605,.F.);
#4857=ORIENTED_EDGE('',*,*,#3602,.F.);
#4858=ORIENTED_EDGE('',*,*,#3606,.F.);
#4859=ORIENTED_EDGE('',*,*,#3607,.F.);
#4860=ORIENTED_EDGE('',*,*,#3606,.T.);
#4861=ORIENTED_EDGE('',*,*,#3601,.T.);
#4862=ORIENTED_EDGE('',*,*,#3608,.F.);
#4863=ORIENTED_EDGE('',*,*,#3609,.F.);
#4864=ORIENTED_EDGE('',*,*,#3610,.F.);
#4865=ORIENTED_EDGE('',*,*,#3607,.T.);
#4866=ORIENTED_EDGE('',*,*,#3609,.T.);
#4867=ORIENTED_EDGE('',*,*,#3611,.F.);
#4868=ORIENTED_EDGE('',*,*,#3612,.F.);
#4869=ORIENTED_EDGE('',*,*,#3603,.T.);
#4870=ORIENTED_EDGE('',*,*,#3575,.F.);
#4871=ORIENTED_EDGE('',*,*,#3613,.F.);
#4872=ORIENTED_EDGE('',*,*,#3604,.T.);
#4873=ORIENTED_EDGE('',*,*,#3612,.T.);
#4874=ORIENTED_EDGE('',*,*,#3614,.F.);
#4875=ORIENTED_EDGE('',*,*,#3599,.F.);
#4876=ORIENTED_EDGE('',*,*,#3600,.T.);
#4877=ORIENTED_EDGE('',*,*,#3614,.T.);
#4878=ORIENTED_EDGE('',*,*,#3611,.T.);
#4879=ORIENTED_EDGE('',*,*,#3608,.T.);
#4880=ORIENTED_EDGE('',*,*,#3507,.T.);
#4881=ORIENTED_EDGE('',*,*,#3448,.T.);
#4882=ORIENTED_EDGE('',*,*,#3504,.T.);
#4883=ORIENTED_EDGE('',*,*,#3498,.T.);
#4884=ORIENTED_EDGE('',*,*,#3515,.T.);
#4885=ORIENTED_EDGE('',*,*,#3348,.T.);
#4886=ORIENTED_EDGE('',*,*,#3512,.T.);
#4887=ORIENTED_EDGE('',*,*,#3398,.T.);
#4888=ORIENTED_EDGE('',*,*,#3597,.T.);
#4889=ORIENTED_EDGE('',*,*,#3615,.T.);
#4890=ORIENTED_EDGE('',*,*,#3616,.T.);
#4891=ORIENTED_EDGE('',*,*,#3578,.T.);
#4892=ORIENTED_EDGE('',*,*,#3580,.T.);
#4893=ORIENTED_EDGE('',*,*,#3587,.T.);
#4894=ORIENTED_EDGE('',*,*,#3585,.T.);
#4895=ORIENTED_EDGE('',*,*,#3583,.T.);
#4896=ORIENTED_EDGE('',*,*,#3613,.T.);
#4897=ORIENTED_EDGE('',*,*,#3574,.T.);
#4898=ORIENTED_EDGE('',*,*,#3617,.T.);
#4899=ORIENTED_EDGE('',*,*,#3618,.T.);
#4900=ORIENTED_EDGE('',*,*,#3588,.T.);
#4901=ORIENTED_EDGE('',*,*,#3595,.T.);
#4902=ORIENTED_EDGE('',*,*,#3593,.T.);
#4903=ORIENTED_EDGE('',*,*,#3591,.T.);
#4904=ORIENTED_EDGE('',*,*,#3560,.T.);
#4905=ORIENTED_EDGE('',*,*,#3619,.T.);
#4906=ORIENTED_EDGE('',*,*,#3615,.F.);
#4907=ORIENTED_EDGE('',*,*,#3596,.T.);
#4908=ORIENTED_EDGE('',*,*,#3605,.T.);
#4909=ORIENTED_EDGE('',*,*,#3610,.T.);
#4910=ORIENTED_EDGE('',*,*,#3618,.F.);
#4911=ORIENTED_EDGE('',*,*,#3620,.F.);
#4912=ORIENTED_EDGE('',*,*,#3552,.T.);
#4913=ORIENTED_EDGE('',*,*,#3550,.F.);
#4914=ORIENTED_EDGE('',*,*,#3551,.T.);
#4915=ORIENTED_EDGE('',*,*,#3546,.T.);
#4916=ORIENTED_EDGE('',*,*,#3522,.T.);
#4917=ORIENTED_EDGE('',*,*,#3553,.T.);
#4918=ORIENTED_EDGE('',*,*,#3620,.T.);
#4919=ORIENTED_EDGE('',*,*,#3617,.F.);
#4920=ORIENTED_EDGE('',*,*,#3573,.F.);
#4921=ORIENTED_EDGE('',*,*,#3559,.T.);
#4922=ORIENTED_EDGE('',*,*,#3579,.T.);
#4923=ORIENTED_EDGE('',*,*,#3616,.F.);
#4924=ORIENTED_EDGE('',*,*,#3619,.F.);
#4925=ORIENTED_EDGE('',*,*,#3621,.T.);
#4926=ORIENTED_EDGE('',*,*,#3622,.T.);
#4927=ORIENTED_EDGE('',*,*,#3623,.F.);
#4928=ORIENTED_EDGE('',*,*,#3624,.T.);
#4929=ORIENTED_EDGE('',*,*,#3625,.T.);
#4930=ORIENTED_EDGE('',*,*,#3626,.T.);
#4931=ORIENTED_EDGE('',*,*,#3621,.F.);
#4932=ORIENTED_EDGE('',*,*,#3627,.T.);
#4933=ORIENTED_EDGE('',*,*,#3628,.T.);
#4934=ORIENTED_EDGE('',*,*,#3629,.T.);
#4935=ORIENTED_EDGE('',*,*,#3625,.F.);
#4936=ORIENTED_EDGE('',*,*,#3630,.T.);
#4937=ORIENTED_EDGE('',*,*,#3631,.T.);
#4938=ORIENTED_EDGE('',*,*,#3632,.T.);
#4939=ORIENTED_EDGE('',*,*,#3628,.F.);
#4940=ORIENTED_EDGE('',*,*,#3633,.T.);
#4941=ORIENTED_EDGE('',*,*,#3634,.T.);
#4942=ORIENTED_EDGE('',*,*,#3635,.T.);
#4943=ORIENTED_EDGE('',*,*,#3631,.F.);
#4944=ORIENTED_EDGE('',*,*,#3636,.T.);
#4945=ORIENTED_EDGE('',*,*,#3637,.T.);
#4946=ORIENTED_EDGE('',*,*,#3638,.T.);
#4947=ORIENTED_EDGE('',*,*,#3634,.F.);
#4948=ORIENTED_EDGE('',*,*,#3639,.T.);
#4949=ORIENTED_EDGE('',*,*,#3640,.T.);
#4950=ORIENTED_EDGE('',*,*,#3641,.T.);
#4951=ORIENTED_EDGE('',*,*,#3637,.F.);
#4952=ORIENTED_EDGE('',*,*,#3642,.T.);
#4953=ORIENTED_EDGE('',*,*,#3643,.T.);
#4954=ORIENTED_EDGE('',*,*,#3644,.T.);
#4955=ORIENTED_EDGE('',*,*,#3640,.F.);
#4956=ORIENTED_EDGE('',*,*,#3645,.T.);
#4957=ORIENTED_EDGE('',*,*,#3646,.T.);
#4958=ORIENTED_EDGE('',*,*,#3647,.T.);
#4959=ORIENTED_EDGE('',*,*,#3643,.F.);
#4960=ORIENTED_EDGE('',*,*,#3648,.T.);
#4961=ORIENTED_EDGE('',*,*,#3649,.F.);
#4962=ORIENTED_EDGE('',*,*,#3650,.T.);
#4963=ORIENTED_EDGE('',*,*,#3651,.F.);
#4964=ORIENTED_EDGE('',*,*,#3652,.T.);
#4965=ORIENTED_EDGE('',*,*,#3653,.T.);
#4966=ORIENTED_EDGE('',*,*,#3654,.T.);
#4967=ORIENTED_EDGE('',*,*,#3655,.F.);
#4968=ORIENTED_EDGE('',*,*,#3656,.F.);
#4969=ORIENTED_EDGE('',*,*,#3657,.T.);
#4970=ORIENTED_EDGE('',*,*,#3658,.T.);
#4971=ORIENTED_EDGE('',*,*,#3653,.F.);
#4972=ORIENTED_EDGE('',*,*,#3659,.F.);
#4973=ORIENTED_EDGE('',*,*,#3660,.T.);
#4974=ORIENTED_EDGE('',*,*,#3661,.T.);
#4975=ORIENTED_EDGE('',*,*,#3657,.F.);
#4976=ORIENTED_EDGE('',*,*,#3662,.F.);
#4977=ORIENTED_EDGE('',*,*,#3663,.T.);
#4978=ORIENTED_EDGE('',*,*,#3664,.T.);
#4979=ORIENTED_EDGE('',*,*,#3660,.F.);
#4980=ORIENTED_EDGE('',*,*,#3665,.F.);
#4981=ORIENTED_EDGE('',*,*,#3666,.T.);
#4982=ORIENTED_EDGE('',*,*,#3667,.T.);
#4983=ORIENTED_EDGE('',*,*,#3663,.F.);
#4984=ORIENTED_EDGE('',*,*,#3668,.F.);
#4985=ORIENTED_EDGE('',*,*,#3669,.T.);
#4986=ORIENTED_EDGE('',*,*,#3670,.T.);
#4987=ORIENTED_EDGE('',*,*,#3666,.F.);
#4988=ORIENTED_EDGE('',*,*,#3671,.F.);
#4989=ORIENTED_EDGE('',*,*,#3672,.T.);
#4990=ORIENTED_EDGE('',*,*,#3673,.T.);
#4991=ORIENTED_EDGE('',*,*,#3669,.F.);
#4992=ORIENTED_EDGE('',*,*,#3674,.F.);
#4993=ORIENTED_EDGE('',*,*,#3675,.T.);
#4994=ORIENTED_EDGE('',*,*,#3676,.T.);
#4995=ORIENTED_EDGE('',*,*,#3672,.F.);
#4996=ORIENTED_EDGE('',*,*,#3677,.F.);
#4997=ORIENTED_EDGE('',*,*,#3678,.T.);
#4998=ORIENTED_EDGE('',*,*,#3679,.T.);
#4999=ORIENTED_EDGE('',*,*,#3675,.F.);
#5000=ORIENTED_EDGE('',*,*,#3680,.F.);
#5001=ORIENTED_EDGE('',*,*,#3681,.F.);
#5002=ORIENTED_EDGE('',*,*,#3682,.F.);
#5003=ORIENTED_EDGE('',*,*,#3683,.F.);
#5004=ORIENTED_EDGE('',*,*,#3684,.T.);
#5005=ORIENTED_EDGE('',*,*,#3685,.F.);
#5006=ORIENTED_EDGE('',*,*,#3686,.T.);
#5007=ORIENTED_EDGE('',*,*,#3687,.F.);
#5008=ORIENTED_EDGE('',*,*,#3688,.F.);
#5009=ORIENTED_EDGE('',*,*,#3689,.F.);
#5010=ORIENTED_EDGE('',*,*,#3690,.T.);
#5011=ORIENTED_EDGE('',*,*,#3691,.F.);
#5012=ORIENTED_EDGE('',*,*,#3686,.F.);
#5013=ORIENTED_EDGE('',*,*,#3692,.F.);
#5014=ORIENTED_EDGE('',*,*,#3693,.T.);
#5015=ORIENTED_EDGE('',*,*,#3694,.F.);
#5016=ORIENTED_EDGE('',*,*,#3690,.F.);
#5017=ORIENTED_EDGE('',*,*,#3695,.F.);
#5018=ORIENTED_EDGE('',*,*,#3688,.T.);
#5019=ORIENTED_EDGE('',*,*,#3696,.F.);
#5020=ORIENTED_EDGE('',*,*,#3693,.F.);
#5021=ORIENTED_EDGE('',*,*,#3681,.T.);
#5022=ORIENTED_EDGE('',*,*,#3697,.T.);
#5023=ORIENTED_EDGE('',*,*,#3678,.F.);
#5024=ORIENTED_EDGE('',*,*,#3698,.F.);
#5025=ORIENTED_EDGE('',*,*,#3699,.F.);
#5026=ORIENTED_EDGE('',*,*,#3654,.F.);
#5027=ORIENTED_EDGE('',*,*,#3658,.F.);
#5028=ORIENTED_EDGE('',*,*,#3661,.F.);
#5029=ORIENTED_EDGE('',*,*,#3664,.F.);
#5030=ORIENTED_EDGE('',*,*,#3667,.F.);
#5031=ORIENTED_EDGE('',*,*,#3670,.F.);
#5032=ORIENTED_EDGE('',*,*,#3673,.F.);
#5033=ORIENTED_EDGE('',*,*,#3676,.F.);
#5034=ORIENTED_EDGE('',*,*,#3679,.F.);
#5035=ORIENTED_EDGE('',*,*,#3697,.F.);
#5036=ORIENTED_EDGE('',*,*,#3684,.F.);
#5037=ORIENTED_EDGE('',*,*,#3700,.F.);
#5038=ORIENTED_EDGE('',*,*,#3650,.F.);
#5039=ORIENTED_EDGE('',*,*,#3701,.F.);
#5040=ORIENTED_EDGE('',*,*,#3648,.F.);
#5041=ORIENTED_EDGE('',*,*,#3645,.F.);
#5042=ORIENTED_EDGE('',*,*,#3642,.F.);
#5043=ORIENTED_EDGE('',*,*,#3639,.F.);
#5044=ORIENTED_EDGE('',*,*,#3636,.F.);
#5045=ORIENTED_EDGE('',*,*,#3633,.F.);
#5046=ORIENTED_EDGE('',*,*,#3630,.F.);
#5047=ORIENTED_EDGE('',*,*,#3627,.F.);
#5048=ORIENTED_EDGE('',*,*,#3624,.F.);
#5049=ORIENTED_EDGE('',*,*,#3702,.F.);
#5050=ORIENTED_EDGE('',*,*,#3622,.F.);
#5051=ORIENTED_EDGE('',*,*,#3626,.F.);
#5052=ORIENTED_EDGE('',*,*,#3629,.F.);
#5053=ORIENTED_EDGE('',*,*,#3632,.F.);
#5054=ORIENTED_EDGE('',*,*,#3635,.F.);
#5055=ORIENTED_EDGE('',*,*,#3638,.F.);
#5056=ORIENTED_EDGE('',*,*,#3641,.F.);
#5057=ORIENTED_EDGE('',*,*,#3644,.F.);
#5058=ORIENTED_EDGE('',*,*,#3647,.F.);
#5059=ORIENTED_EDGE('',*,*,#3703,.F.);
#5060=ORIENTED_EDGE('',*,*,#3652,.F.);
#5061=ORIENTED_EDGE('',*,*,#3704,.F.);
#5062=ORIENTED_EDGE('',*,*,#3682,.T.);
#5063=ORIENTED_EDGE('',*,*,#3698,.T.);
#5064=ORIENTED_EDGE('',*,*,#3680,.T.);
#5065=ORIENTED_EDGE('',*,*,#3677,.T.);
#5066=ORIENTED_EDGE('',*,*,#3674,.T.);
#5067=ORIENTED_EDGE('',*,*,#3671,.T.);
#5068=ORIENTED_EDGE('',*,*,#3668,.T.);
#5069=ORIENTED_EDGE('',*,*,#3665,.T.);
#5070=ORIENTED_EDGE('',*,*,#3662,.T.);
#5071=ORIENTED_EDGE('',*,*,#3659,.T.);
#5072=ORIENTED_EDGE('',*,*,#3656,.T.);
#5073=ORIENTED_EDGE('',*,*,#3705,.T.);
#5074=ORIENTED_EDGE('',*,*,#3700,.T.);
#5075=ORIENTED_EDGE('',*,*,#3683,.T.);
#5076=ORIENTED_EDGE('',*,*,#3704,.T.);
#5077=ORIENTED_EDGE('',*,*,#3651,.T.);
#5078=ORIENTED_EDGE('',*,*,#3649,.T.);
#5079=ORIENTED_EDGE('',*,*,#3703,.T.);
#5080=ORIENTED_EDGE('',*,*,#3646,.F.);
#5081=ORIENTED_EDGE('',*,*,#3701,.T.);
#5082=ORIENTED_EDGE('',*,*,#3706,.F.);
#5083=ORIENTED_EDGE('',*,*,#3707,.T.);
#5084=ORIENTED_EDGE('',*,*,#3708,.F.);
#5085=ORIENTED_EDGE('',*,*,#3707,.F.);
#5086=ORIENTED_EDGE('',*,*,#3709,.F.);
#5087=ORIENTED_EDGE('',*,*,#3710,.T.);
#5088=ORIENTED_EDGE('',*,*,#3711,.F.);
#5089=ORIENTED_EDGE('',*,*,#3710,.F.);
#5090=ORIENTED_EDGE('',*,*,#3712,.F.);
#5091=ORIENTED_EDGE('',*,*,#3713,.T.);
#5092=ORIENTED_EDGE('',*,*,#3714,.F.);
#5093=ORIENTED_EDGE('',*,*,#3713,.F.);
#5094=ORIENTED_EDGE('',*,*,#3705,.F.);
#5095=ORIENTED_EDGE('',*,*,#3715,.T.);
#5096=ORIENTED_EDGE('',*,*,#3716,.F.);
#5097=ORIENTED_EDGE('',*,*,#3715,.F.);
#5098=ORIENTED_EDGE('',*,*,#3717,.F.);
#5099=ORIENTED_EDGE('',*,*,#3718,.T.);
#5100=ORIENTED_EDGE('',*,*,#3719,.T.);
#5101=ORIENTED_EDGE('',*,*,#3720,.F.);
#5102=ORIENTED_EDGE('',*,*,#3721,.T.);
#5103=ORIENTED_EDGE('',*,*,#3722,.T.);
#5104=ORIENTED_EDGE('',*,*,#3723,.T.);
#5105=ORIENTED_EDGE('',*,*,#3724,.T.);
#5106=ORIENTED_EDGE('',*,*,#3725,.T.);
#5107=ORIENTED_EDGE('',*,*,#3726,.T.);
#5108=ORIENTED_EDGE('',*,*,#3727,.T.);
#5109=ORIENTED_EDGE('',*,*,#3728,.T.);
#5110=ORIENTED_EDGE('',*,*,#3729,.T.);
#5111=ORIENTED_EDGE('',*,*,#3720,.T.);
#5112=ORIENTED_EDGE('',*,*,#3685,.T.);
#5113=ORIENTED_EDGE('',*,*,#3695,.T.);
#5114=ORIENTED_EDGE('',*,*,#3692,.T.);
#5115=ORIENTED_EDGE('',*,*,#3689,.T.);
#5116=ORIENTED_EDGE('',*,*,#3706,.T.);
#5117=ORIENTED_EDGE('',*,*,#3709,.T.);
#5118=ORIENTED_EDGE('',*,*,#3712,.T.);
#5119=ORIENTED_EDGE('',*,*,#3716,.T.);
#5120=ORIENTED_EDGE('',*,*,#3730,.F.);
#5121=ORIENTED_EDGE('',*,*,#3731,.T.);
#5122=ORIENTED_EDGE('',*,*,#3717,.T.);
#5123=ORIENTED_EDGE('',*,*,#3729,.F.);
#5124=ORIENTED_EDGE('',*,*,#3732,.F.);
#5125=ORIENTED_EDGE('',*,*,#3721,.F.);
#5126=ORIENTED_EDGE('',*,*,#3719,.F.);
#5127=ORIENTED_EDGE('',*,*,#3733,.T.);
#5128=ORIENTED_EDGE('',*,*,#3732,.T.);
#5129=ORIENTED_EDGE('',*,*,#3734,.T.);
#5130=ORIENTED_EDGE('',*,*,#3735,.T.);
#5131=ORIENTED_EDGE('',*,*,#3722,.F.);
#5132=ORIENTED_EDGE('',*,*,#3731,.F.);
#5133=ORIENTED_EDGE('',*,*,#3736,.F.);
#5134=ORIENTED_EDGE('',*,*,#3737,.F.);
#5135=ORIENTED_EDGE('',*,*,#3738,.F.);
#5136=ORIENTED_EDGE('',*,*,#3739,.F.);
#5137=ORIENTED_EDGE('',*,*,#3740,.F.);
#5138=ORIENTED_EDGE('',*,*,#3741,.F.);
#5139=ORIENTED_EDGE('',*,*,#3734,.F.);
#5140=ORIENTED_EDGE('',*,*,#3733,.F.);
#5141=ORIENTED_EDGE('',*,*,#3718,.F.);
#5142=ORIENTED_EDGE('',*,*,#3687,.T.);
#5143=ORIENTED_EDGE('',*,*,#3691,.T.);
#5144=ORIENTED_EDGE('',*,*,#3694,.T.);
#5145=ORIENTED_EDGE('',*,*,#3696,.T.);
#5146=ORIENTED_EDGE('',*,*,#3699,.T.);
#5147=ORIENTED_EDGE('',*,*,#3623,.T.);
#5148=ORIENTED_EDGE('',*,*,#3702,.T.);
#5149=ORIENTED_EDGE('',*,*,#3655,.T.);
#5150=ORIENTED_EDGE('',*,*,#3708,.T.);
#5151=ORIENTED_EDGE('',*,*,#3711,.T.);
#5152=ORIENTED_EDGE('',*,*,#3714,.T.);
#5153=ORIENTED_EDGE('',*,*,#3742,.F.);
#5154=ORIENTED_EDGE('',*,*,#3725,.F.);
#5155=ORIENTED_EDGE('',*,*,#3743,.F.);
#5156=ORIENTED_EDGE('',*,*,#3739,.T.);
#5157=ORIENTED_EDGE('',*,*,#3730,.T.);
#5158=ORIENTED_EDGE('',*,*,#3728,.F.);
#5159=ORIENTED_EDGE('',*,*,#3744,.F.);
#5160=ORIENTED_EDGE('',*,*,#3736,.T.);
#5161=ORIENTED_EDGE('',*,*,#3743,.T.);
#5162=ORIENTED_EDGE('',*,*,#3724,.F.);
#5163=ORIENTED_EDGE('',*,*,#3745,.F.);
#5164=ORIENTED_EDGE('',*,*,#3740,.T.);
#5165=ORIENTED_EDGE('',*,*,#3737,.T.);
#5166=ORIENTED_EDGE('',*,*,#3744,.T.);
#5167=ORIENTED_EDGE('',*,*,#3727,.F.);
#5168=ORIENTED_EDGE('',*,*,#3746,.F.);
#5169=ORIENTED_EDGE('',*,*,#3742,.T.);
#5170=ORIENTED_EDGE('',*,*,#3738,.T.);
#5171=ORIENTED_EDGE('',*,*,#3746,.T.);
#5172=ORIENTED_EDGE('',*,*,#3726,.F.);
#5173=ORIENTED_EDGE('',*,*,#3741,.T.);
#5174=ORIENTED_EDGE('',*,*,#3745,.T.);
#5175=ORIENTED_EDGE('',*,*,#3723,.F.);
#5176=ORIENTED_EDGE('',*,*,#3735,.F.);
#5177=ORIENTED_EDGE('',*,*,#3747,.T.);
#5178=ORIENTED_EDGE('',*,*,#3748,.F.);
#5179=ORIENTED_EDGE('',*,*,#3749,.T.);
#5180=ORIENTED_EDGE('',*,*,#3750,.F.);
#5181=ORIENTED_EDGE('',*,*,#3749,.F.);
#5182=ORIENTED_EDGE('',*,*,#3751,.F.);
#5183=ORIENTED_EDGE('',*,*,#3752,.T.);
#5184=ORIENTED_EDGE('',*,*,#3753,.F.);
#5185=ORIENTED_EDGE('',*,*,#3752,.F.);
#5186=ORIENTED_EDGE('',*,*,#3754,.F.);
#5187=ORIENTED_EDGE('',*,*,#3755,.T.);
#5188=ORIENTED_EDGE('',*,*,#3756,.F.);
#5189=ORIENTED_EDGE('',*,*,#3755,.F.);
#5190=ORIENTED_EDGE('',*,*,#3757,.F.);
#5191=ORIENTED_EDGE('',*,*,#3747,.F.);
#5192=ORIENTED_EDGE('',*,*,#3758,.F.);
#5193=ORIENTED_EDGE('',*,*,#3759,.T.);
#5194=ORIENTED_EDGE('',*,*,#3760,.F.);
#5195=ORIENTED_EDGE('',*,*,#3761,.F.);
#5196=ORIENTED_EDGE('',*,*,#3762,.F.);
#5197=ORIENTED_EDGE('',*,*,#3763,.T.);
#5198=ORIENTED_EDGE('',*,*,#3764,.F.);
#5199=ORIENTED_EDGE('',*,*,#3765,.F.);
#5200=ORIENTED_EDGE('',*,*,#3766,.F.);
#5201=ORIENTED_EDGE('',*,*,#3765,.T.);
#5202=ORIENTED_EDGE('',*,*,#3767,.T.);
#5203=ORIENTED_EDGE('',*,*,#3768,.F.);
#5204=ORIENTED_EDGE('',*,*,#3769,.F.);
#5205=ORIENTED_EDGE('',*,*,#3760,.T.);
#5206=ORIENTED_EDGE('',*,*,#3770,.F.);
#5207=ORIENTED_EDGE('',*,*,#3766,.T.);
#5208=ORIENTED_EDGE('',*,*,#3769,.T.);
#5209=ORIENTED_EDGE('',*,*,#3771,.F.);
#5210=ORIENTED_EDGE('',*,*,#3772,.F.);
#5211=ORIENTED_EDGE('',*,*,#3761,.T.);
#5212=ORIENTED_EDGE('',*,*,#3772,.T.);
#5213=ORIENTED_EDGE('',*,*,#3773,.F.);
#5214=ORIENTED_EDGE('',*,*,#3774,.F.);
#5215=ORIENTED_EDGE('',*,*,#3764,.T.);
#5216=ORIENTED_EDGE('',*,*,#3775,.F.);
#5217=ORIENTED_EDGE('',*,*,#3762,.T.);
#5218=ORIENTED_EDGE('',*,*,#3774,.T.);
#5219=ORIENTED_EDGE('',*,*,#3776,.F.);
#5220=ORIENTED_EDGE('',*,*,#3767,.F.);
#5221=ORIENTED_EDGE('',*,*,#3776,.T.);
#5222=ORIENTED_EDGE('',*,*,#3773,.T.);
#5223=ORIENTED_EDGE('',*,*,#3771,.T.);
#5224=ORIENTED_EDGE('',*,*,#3768,.T.);
#5225=ORIENTED_EDGE('',*,*,#3775,.T.);
#5226=ORIENTED_EDGE('',*,*,#3777,.T.);
#5227=ORIENTED_EDGE('',*,*,#3778,.T.);
#5228=ORIENTED_EDGE('',*,*,#3779,.T.);
#5229=ORIENTED_EDGE('',*,*,#3770,.T.);
#5230=ORIENTED_EDGE('',*,*,#3780,.T.);
#5231=ORIENTED_EDGE('',*,*,#3781,.T.);
#5232=ORIENTED_EDGE('',*,*,#3782,.T.);
#5233=ORIENTED_EDGE('',*,*,#3783,.F.);
#5234=ORIENTED_EDGE('',*,*,#3784,.T.);
#5235=ORIENTED_EDGE('',*,*,#3781,.F.);
#5236=ORIENTED_EDGE('',*,*,#3785,.F.);
#5237=ORIENTED_EDGE('',*,*,#3786,.F.);
#5238=ORIENTED_EDGE('',*,*,#3787,.T.);
#5239=ORIENTED_EDGE('',*,*,#3778,.F.);
#5240=ORIENTED_EDGE('',*,*,#3788,.F.);
#5241=ORIENTED_EDGE('',*,*,#3786,.T.);
#5242=ORIENTED_EDGE('',*,*,#3789,.T.);
#5243=ORIENTED_EDGE('',*,*,#3790,.T.);
#5244=ORIENTED_EDGE('',*,*,#3791,.T.);
#5245=ORIENTED_EDGE('',*,*,#3792,.T.);
#5246=ORIENTED_EDGE('',*,*,#3793,.T.);
#5247=ORIENTED_EDGE('',*,*,#3789,.F.);
#5248=ORIENTED_EDGE('',*,*,#3788,.T.);
#5249=ORIENTED_EDGE('',*,*,#3777,.F.);
#5250=ORIENTED_EDGE('',*,*,#3763,.F.);
#5251=ORIENTED_EDGE('',*,*,#3782,.F.);
#5252=ORIENTED_EDGE('',*,*,#3784,.F.);
#5253=ORIENTED_EDGE('',*,*,#3794,.F.);
#5254=ORIENTED_EDGE('',*,*,#3795,.F.);
#5255=ORIENTED_EDGE('',*,*,#3750,.T.);
#5256=ORIENTED_EDGE('',*,*,#3753,.T.);
#5257=ORIENTED_EDGE('',*,*,#3756,.T.);
#5258=ORIENTED_EDGE('',*,*,#3758,.T.);
#5259=ORIENTED_EDGE('',*,*,#3796,.T.);
#5260=ORIENTED_EDGE('',*,*,#3795,.T.);
#5261=ORIENTED_EDGE('',*,*,#3797,.F.);
#5262=ORIENTED_EDGE('',*,*,#3798,.F.);
#5263=ORIENTED_EDGE('',*,*,#3799,.T.);
#5264=ORIENTED_EDGE('',*,*,#3798,.T.);
#5265=ORIENTED_EDGE('',*,*,#3800,.F.);
#5266=ORIENTED_EDGE('',*,*,#3785,.T.);
#5267=ORIENTED_EDGE('',*,*,#3780,.F.);
#5268=ORIENTED_EDGE('',*,*,#3759,.F.);
#5269=ORIENTED_EDGE('',*,*,#3779,.F.);
#5270=ORIENTED_EDGE('',*,*,#3787,.F.);
#5271=ORIENTED_EDGE('',*,*,#3791,.F.);
#5272=ORIENTED_EDGE('',*,*,#3801,.F.);
#5273=ORIENTED_EDGE('',*,*,#3748,.T.);
#5274=ORIENTED_EDGE('',*,*,#3757,.T.);
#5275=ORIENTED_EDGE('',*,*,#3754,.T.);
#5276=ORIENTED_EDGE('',*,*,#3751,.T.);
#5277=ORIENTED_EDGE('',*,*,#3802,.T.);
#5278=ORIENTED_EDGE('',*,*,#3801,.T.);
#5279=ORIENTED_EDGE('',*,*,#3790,.F.);
#5280=ORIENTED_EDGE('',*,*,#3793,.F.);
#5281=ORIENTED_EDGE('',*,*,#3783,.T.);
#5282=ORIENTED_EDGE('',*,*,#3800,.T.);
#5283=ORIENTED_EDGE('',*,*,#3797,.T.);
#5284=ORIENTED_EDGE('',*,*,#3794,.T.);
#5285=ORIENTED_EDGE('',*,*,#3802,.F.);
#5286=ORIENTED_EDGE('',*,*,#3792,.F.);
#5287=ORIENTED_EDGE('',*,*,#3796,.F.);
#5288=ORIENTED_EDGE('',*,*,#3799,.F.);
#5289=ORIENTED_EDGE('',*,*,#3803,.T.);
#5290=ORIENTED_EDGE('',*,*,#3804,.T.);
#5291=ORIENTED_EDGE('',*,*,#3805,.F.);
#5292=ORIENTED_EDGE('',*,*,#3804,.F.);
#5293=ORIENTED_EDGE('',*,*,#3806,.F.);
#5294=ORIENTED_EDGE('',*,*,#3803,.F.);
#5295=ORIENTED_EDGE('',*,*,#3807,.F.);
#5296=ORIENTED_EDGE('',*,*,#3805,.T.);
#5297=ORIENTED_EDGE('',*,*,#3808,.F.);
#5298=ORIENTED_EDGE('',*,*,#3809,.T.);
#5299=ORIENTED_EDGE('',*,*,#3807,.T.);
#5300=ORIENTED_EDGE('',*,*,#3809,.F.);
#5301=ORIENTED_EDGE('',*,*,#3810,.T.);
#5302=ORIENTED_EDGE('',*,*,#3811,.F.);
#5303=ORIENTED_EDGE('',*,*,#3810,.F.);
#5304=ORIENTED_EDGE('',*,*,#3812,.T.);
#5305=ORIENTED_EDGE('',*,*,#3813,.T.);
#5306=ORIENTED_EDGE('',*,*,#3812,.F.);
#5307=ORIENTED_EDGE('',*,*,#3813,.F.);
#5308=ORIENTED_EDGE('',*,*,#3806,.T.);
#5309=ORIENTED_EDGE('',*,*,#3814,.T.);
#5310=ORIENTED_EDGE('',*,*,#3811,.T.);
#5311=ORIENTED_EDGE('',*,*,#3814,.F.);
#5312=ORIENTED_EDGE('',*,*,#3808,.T.);
#5313=ORIENTED_EDGE('',*,*,#3815,.T.);
#5314=ORIENTED_EDGE('',*,*,#3816,.T.);
#5315=ORIENTED_EDGE('',*,*,#3817,.F.);
#5316=ORIENTED_EDGE('',*,*,#3816,.F.);
#5317=ORIENTED_EDGE('',*,*,#3818,.F.);
#5318=ORIENTED_EDGE('',*,*,#3815,.F.);
#5319=ORIENTED_EDGE('',*,*,#3819,.F.);
#5320=ORIENTED_EDGE('',*,*,#3817,.T.);
#5321=ORIENTED_EDGE('',*,*,#3820,.F.);
#5322=ORIENTED_EDGE('',*,*,#3821,.T.);
#5323=ORIENTED_EDGE('',*,*,#3819,.T.);
#5324=ORIENTED_EDGE('',*,*,#3821,.F.);
#5325=ORIENTED_EDGE('',*,*,#3822,.T.);
#5326=ORIENTED_EDGE('',*,*,#3823,.F.);
#5327=ORIENTED_EDGE('',*,*,#3822,.F.);
#5328=ORIENTED_EDGE('',*,*,#3824,.T.);
#5329=ORIENTED_EDGE('',*,*,#3825,.T.);
#5330=ORIENTED_EDGE('',*,*,#3824,.F.);
#5331=ORIENTED_EDGE('',*,*,#3825,.F.);
#5332=ORIENTED_EDGE('',*,*,#3818,.T.);
#5333=ORIENTED_EDGE('',*,*,#3826,.T.);
#5334=ORIENTED_EDGE('',*,*,#3823,.T.);
#5335=ORIENTED_EDGE('',*,*,#3826,.F.);
#5336=ORIENTED_EDGE('',*,*,#3820,.T.);
#5337=ORIENTED_EDGE('',*,*,#3827,.F.);
#5338=ORIENTED_EDGE('',*,*,#3828,.T.);
#5339=ORIENTED_EDGE('',*,*,#3829,.T.);
#5340=ORIENTED_EDGE('',*,*,#3828,.F.);
#5341=ORIENTED_EDGE('',*,*,#3830,.F.);
#5342=ORIENTED_EDGE('',*,*,#3831,.T.);
#5343=ORIENTED_EDGE('',*,*,#3832,.T.);
#5344=ORIENTED_EDGE('',*,*,#3831,.F.);
#5345=ORIENTED_EDGE('',*,*,#3830,.T.);
#5346=ORIENTED_EDGE('',*,*,#3827,.T.);
#5347=ORIENTED_EDGE('',*,*,#3832,.F.);
#5348=ORIENTED_EDGE('',*,*,#3829,.F.);
#5349=ORIENTED_EDGE('',*,*,#3833,.F.);
#5350=ORIENTED_EDGE('',*,*,#3834,.F.);
#5351=ORIENTED_EDGE('',*,*,#3835,.F.);
#5352=ORIENTED_EDGE('',*,*,#3836,.F.);
#5353=ORIENTED_EDGE('',*,*,#3837,.F.);
#5354=ORIENTED_EDGE('',*,*,#3838,.F.);
#5355=ORIENTED_EDGE('',*,*,#3839,.F.);
#5356=ORIENTED_EDGE('',*,*,#3840,.F.);
#5357=ORIENTED_EDGE('',*,*,#3840,.T.);
#5358=ORIENTED_EDGE('',*,*,#3841,.F.);
#5359=ORIENTED_EDGE('',*,*,#3834,.T.);
#5360=ORIENTED_EDGE('',*,*,#3842,.F.);
#5361=ORIENTED_EDGE('',*,*,#3837,.T.);
#5362=ORIENTED_EDGE('',*,*,#3842,.T.);
#5363=ORIENTED_EDGE('',*,*,#3833,.T.);
#5364=ORIENTED_EDGE('',*,*,#3843,.F.);
#5365=ORIENTED_EDGE('',*,*,#3839,.T.);
#5366=ORIENTED_EDGE('',*,*,#3844,.F.);
#5367=ORIENTED_EDGE('',*,*,#3835,.T.);
#5368=ORIENTED_EDGE('',*,*,#3841,.T.);
#5369=ORIENTED_EDGE('',*,*,#3838,.T.);
#5370=ORIENTED_EDGE('',*,*,#3843,.T.);
#5371=ORIENTED_EDGE('',*,*,#3836,.T.);
#5372=ORIENTED_EDGE('',*,*,#3844,.T.);
#5373=ORIENTED_EDGE('',*,*,#3845,.F.);
#5374=ORIENTED_EDGE('',*,*,#3846,.T.);
#5375=ORIENTED_EDGE('',*,*,#3847,.T.);
#5376=ORIENTED_EDGE('',*,*,#3846,.F.);
#5377=ORIENTED_EDGE('',*,*,#3848,.F.);
#5378=ORIENTED_EDGE('',*,*,#3849,.T.);
#5379=ORIENTED_EDGE('',*,*,#3850,.T.);
#5380=ORIENTED_EDGE('',*,*,#3849,.F.);
#5381=ORIENTED_EDGE('',*,*,#3848,.T.);
#5382=ORIENTED_EDGE('',*,*,#3845,.T.);
#5383=ORIENTED_EDGE('',*,*,#3850,.F.);
#5384=ORIENTED_EDGE('',*,*,#3847,.F.);
#5385=ORIENTED_EDGE('',*,*,#3851,.F.);
#5386=ORIENTED_EDGE('',*,*,#3852,.T.);
#5387=ORIENTED_EDGE('',*,*,#3853,.T.);
#5388=ORIENTED_EDGE('',*,*,#3852,.F.);
#5389=ORIENTED_EDGE('',*,*,#3854,.F.);
#5390=ORIENTED_EDGE('',*,*,#3855,.T.);
#5391=ORIENTED_EDGE('',*,*,#3856,.T.);
#5392=ORIENTED_EDGE('',*,*,#3855,.F.);
#5393=ORIENTED_EDGE('',*,*,#3854,.T.);
#5394=ORIENTED_EDGE('',*,*,#3851,.T.);
#5395=ORIENTED_EDGE('',*,*,#3856,.F.);
#5396=ORIENTED_EDGE('',*,*,#3853,.F.);
#5397=ORIENTED_EDGE('',*,*,#3857,.F.);
#5398=ORIENTED_EDGE('',*,*,#3858,.T.);
#5399=ORIENTED_EDGE('',*,*,#3859,.T.);
#5400=ORIENTED_EDGE('',*,*,#3858,.F.);
#5401=ORIENTED_EDGE('',*,*,#3860,.F.);
#5402=ORIENTED_EDGE('',*,*,#3861,.T.);
#5403=ORIENTED_EDGE('',*,*,#3862,.T.);
#5404=ORIENTED_EDGE('',*,*,#3861,.F.);
#5405=ORIENTED_EDGE('',*,*,#3860,.T.);
#5406=ORIENTED_EDGE('',*,*,#3857,.T.);
#5407=ORIENTED_EDGE('',*,*,#3862,.F.);
#5408=ORIENTED_EDGE('',*,*,#3859,.F.);
#5409=ORIENTED_EDGE('',*,*,#3863,.F.);
#5410=ORIENTED_EDGE('',*,*,#3864,.F.);
#5411=ORIENTED_EDGE('',*,*,#3865,.F.);
#5412=ORIENTED_EDGE('',*,*,#3866,.F.);
#5413=ORIENTED_EDGE('',*,*,#3867,.F.);
#5414=ORIENTED_EDGE('',*,*,#3868,.F.);
#5415=ORIENTED_EDGE('',*,*,#3869,.F.);
#5416=ORIENTED_EDGE('',*,*,#3870,.F.);
#5417=ORIENTED_EDGE('',*,*,#3870,.T.);
#5418=ORIENTED_EDGE('',*,*,#3871,.F.);
#5419=ORIENTED_EDGE('',*,*,#3864,.T.);
#5420=ORIENTED_EDGE('',*,*,#3872,.F.);
#5421=ORIENTED_EDGE('',*,*,#3867,.T.);
#5422=ORIENTED_EDGE('',*,*,#3872,.T.);
#5423=ORIENTED_EDGE('',*,*,#3863,.T.);
#5424=ORIENTED_EDGE('',*,*,#3873,.F.);
#5425=ORIENTED_EDGE('',*,*,#3869,.T.);
#5426=ORIENTED_EDGE('',*,*,#3874,.F.);
#5427=ORIENTED_EDGE('',*,*,#3865,.T.);
#5428=ORIENTED_EDGE('',*,*,#3871,.T.);
#5429=ORIENTED_EDGE('',*,*,#3868,.T.);
#5430=ORIENTED_EDGE('',*,*,#3873,.T.);
#5431=ORIENTED_EDGE('',*,*,#3866,.T.);
#5432=ORIENTED_EDGE('',*,*,#3874,.T.);
#5433=ORIENTED_EDGE('',*,*,#3875,.T.);
#5434=ORIENTED_EDGE('',*,*,#3876,.T.);
#5435=ORIENTED_EDGE('',*,*,#3877,.F.);
#5436=ORIENTED_EDGE('',*,*,#3876,.F.);
#5437=ORIENTED_EDGE('',*,*,#3878,.F.);
#5438=ORIENTED_EDGE('',*,*,#3875,.F.);
#5439=ORIENTED_EDGE('',*,*,#3879,.F.);
#5440=ORIENTED_EDGE('',*,*,#3877,.T.);
#5441=ORIENTED_EDGE('',*,*,#3880,.F.);
#5442=ORIENTED_EDGE('',*,*,#3881,.T.);
#5443=ORIENTED_EDGE('',*,*,#3879,.T.);
#5444=ORIENTED_EDGE('',*,*,#3881,.F.);
#5445=ORIENTED_EDGE('',*,*,#3882,.T.);
#5446=ORIENTED_EDGE('',*,*,#3883,.F.);
#5447=ORIENTED_EDGE('',*,*,#3882,.F.);
#5448=ORIENTED_EDGE('',*,*,#3884,.T.);
#5449=ORIENTED_EDGE('',*,*,#3885,.T.);
#5450=ORIENTED_EDGE('',*,*,#3884,.F.);
#5451=ORIENTED_EDGE('',*,*,#3885,.F.);
#5452=ORIENTED_EDGE('',*,*,#3878,.T.);
#5453=ORIENTED_EDGE('',*,*,#3886,.T.);
#5454=ORIENTED_EDGE('',*,*,#3883,.T.);
#5455=ORIENTED_EDGE('',*,*,#3886,.F.);
#5456=ORIENTED_EDGE('',*,*,#3880,.T.);
#5457=ORIENTED_EDGE('',*,*,#3887,.F.);
#5458=ORIENTED_EDGE('',*,*,#3888,.T.);
#5459=ORIENTED_EDGE('',*,*,#3889,.T.);
#5460=ORIENTED_EDGE('',*,*,#3888,.F.);
#5461=ORIENTED_EDGE('',*,*,#3890,.F.);
#5462=ORIENTED_EDGE('',*,*,#3891,.T.);
#5463=ORIENTED_EDGE('',*,*,#3892,.T.);
#5464=ORIENTED_EDGE('',*,*,#3891,.F.);
#5465=ORIENTED_EDGE('',*,*,#3890,.T.);
#5466=ORIENTED_EDGE('',*,*,#3887,.T.);
#5467=ORIENTED_EDGE('',*,*,#3892,.F.);
#5468=ORIENTED_EDGE('',*,*,#3889,.F.);
#5469=ORIENTED_EDGE('',*,*,#3893,.F.);
#5470=ORIENTED_EDGE('',*,*,#3894,.T.);
#5471=ORIENTED_EDGE('',*,*,#3895,.T.);
#5472=ORIENTED_EDGE('',*,*,#3894,.F.);
#5473=ORIENTED_EDGE('',*,*,#3896,.F.);
#5474=ORIENTED_EDGE('',*,*,#3897,.T.);
#5475=ORIENTED_EDGE('',*,*,#3898,.T.);
#5476=ORIENTED_EDGE('',*,*,#3897,.F.);
#5477=ORIENTED_EDGE('',*,*,#3896,.T.);
#5478=ORIENTED_EDGE('',*,*,#3893,.T.);
#5479=ORIENTED_EDGE('',*,*,#3898,.F.);
#5480=ORIENTED_EDGE('',*,*,#3895,.F.);
#5481=ORIENTED_EDGE('',*,*,#3899,.F.);
#5482=ORIENTED_EDGE('',*,*,#3900,.F.);
#5483=ORIENTED_EDGE('',*,*,#3901,.F.);
#5484=ORIENTED_EDGE('',*,*,#3902,.F.);
#5485=ORIENTED_EDGE('',*,*,#3903,.F.);
#5486=ORIENTED_EDGE('',*,*,#3904,.F.);
#5487=ORIENTED_EDGE('',*,*,#3905,.F.);
#5488=ORIENTED_EDGE('',*,*,#3906,.F.);
#5489=ORIENTED_EDGE('',*,*,#3906,.T.);
#5490=ORIENTED_EDGE('',*,*,#3907,.F.);
#5491=ORIENTED_EDGE('',*,*,#3900,.T.);
#5492=ORIENTED_EDGE('',*,*,#3908,.F.);
#5493=ORIENTED_EDGE('',*,*,#3903,.T.);
#5494=ORIENTED_EDGE('',*,*,#3908,.T.);
#5495=ORIENTED_EDGE('',*,*,#3899,.T.);
#5496=ORIENTED_EDGE('',*,*,#3909,.F.);
#5497=ORIENTED_EDGE('',*,*,#3905,.T.);
#5498=ORIENTED_EDGE('',*,*,#3910,.F.);
#5499=ORIENTED_EDGE('',*,*,#3901,.T.);
#5500=ORIENTED_EDGE('',*,*,#3907,.T.);
#5501=ORIENTED_EDGE('',*,*,#3904,.T.);
#5502=ORIENTED_EDGE('',*,*,#3909,.T.);
#5503=ORIENTED_EDGE('',*,*,#3902,.T.);
#5504=ORIENTED_EDGE('',*,*,#3910,.T.);
#5505=ORIENTED_EDGE('',*,*,#3911,.F.);
#5506=ORIENTED_EDGE('',*,*,#3912,.T.);
#5507=ORIENTED_EDGE('',*,*,#3913,.T.);
#5508=ORIENTED_EDGE('',*,*,#3912,.F.);
#5509=ORIENTED_EDGE('',*,*,#3914,.F.);
#5510=ORIENTED_EDGE('',*,*,#3915,.T.);
#5511=ORIENTED_EDGE('',*,*,#3916,.T.);
#5512=ORIENTED_EDGE('',*,*,#3915,.F.);
#5513=ORIENTED_EDGE('',*,*,#3914,.T.);
#5514=ORIENTED_EDGE('',*,*,#3911,.T.);
#5515=ORIENTED_EDGE('',*,*,#3916,.F.);
#5516=ORIENTED_EDGE('',*,*,#3913,.F.);
#5517=ORIENTED_EDGE('',*,*,#3917,.F.);
#5518=ORIENTED_EDGE('',*,*,#3918,.T.);
#5519=ORIENTED_EDGE('',*,*,#3919,.F.);
#5520=ORIENTED_EDGE('',*,*,#3920,.F.);
#5521=ORIENTED_EDGE('',*,*,#3921,.F.);
#5522=ORIENTED_EDGE('',*,*,#3922,.T.);
#5523=ORIENTED_EDGE('',*,*,#3917,.T.);
#5524=ORIENTED_EDGE('',*,*,#3923,.F.);
#5525=ORIENTED_EDGE('',*,*,#3924,.F.);
#5526=ORIENTED_EDGE('',*,*,#3925,.T.);
#5527=ORIENTED_EDGE('',*,*,#3921,.T.);
#5528=ORIENTED_EDGE('',*,*,#3926,.F.);
#5529=ORIENTED_EDGE('',*,*,#3927,.F.);
#5530=ORIENTED_EDGE('',*,*,#3928,.T.);
#5531=ORIENTED_EDGE('',*,*,#3924,.T.);
#5532=ORIENTED_EDGE('',*,*,#3929,.F.);
#5533=ORIENTED_EDGE('',*,*,#3930,.F.);
#5534=ORIENTED_EDGE('',*,*,#3931,.T.);
#5535=ORIENTED_EDGE('',*,*,#3927,.T.);
#5536=ORIENTED_EDGE('',*,*,#3932,.F.);
#5537=ORIENTED_EDGE('',*,*,#3933,.F.);
#5538=ORIENTED_EDGE('',*,*,#3934,.T.);
#5539=ORIENTED_EDGE('',*,*,#3930,.T.);
#5540=ORIENTED_EDGE('',*,*,#3935,.F.);
#5541=ORIENTED_EDGE('',*,*,#3936,.F.);
#5542=ORIENTED_EDGE('',*,*,#3937,.T.);
#5543=ORIENTED_EDGE('',*,*,#3933,.T.);
#5544=ORIENTED_EDGE('',*,*,#3938,.F.);
#5545=ORIENTED_EDGE('',*,*,#3939,.F.);
#5546=ORIENTED_EDGE('',*,*,#3940,.T.);
#5547=ORIENTED_EDGE('',*,*,#3936,.T.);
#5548=ORIENTED_EDGE('',*,*,#3941,.F.);
#5549=ORIENTED_EDGE('',*,*,#3942,.F.);
#5550=ORIENTED_EDGE('',*,*,#3943,.T.);
#5551=ORIENTED_EDGE('',*,*,#3944,.T.);
#5552=ORIENTED_EDGE('',*,*,#3945,.T.);
#5553=ORIENTED_EDGE('',*,*,#3946,.F.);
#5554=ORIENTED_EDGE('',*,*,#3947,.T.);
#5555=ORIENTED_EDGE('',*,*,#3942,.T.);
#5556=ORIENTED_EDGE('',*,*,#3948,.T.);
#5557=ORIENTED_EDGE('',*,*,#3949,.F.);
#5558=ORIENTED_EDGE('',*,*,#3950,.T.);
#5559=ORIENTED_EDGE('',*,*,#3946,.T.);
#5560=ORIENTED_EDGE('',*,*,#3951,.T.);
#5561=ORIENTED_EDGE('',*,*,#3952,.F.);
#5562=ORIENTED_EDGE('',*,*,#3953,.T.);
#5563=ORIENTED_EDGE('',*,*,#3949,.T.);
#5564=ORIENTED_EDGE('',*,*,#3954,.T.);
#5565=ORIENTED_EDGE('',*,*,#3955,.F.);
#5566=ORIENTED_EDGE('',*,*,#3956,.T.);
#5567=ORIENTED_EDGE('',*,*,#3952,.T.);
#5568=ORIENTED_EDGE('',*,*,#3957,.T.);
#5569=ORIENTED_EDGE('',*,*,#3958,.F.);
#5570=ORIENTED_EDGE('',*,*,#3959,.T.);
#5571=ORIENTED_EDGE('',*,*,#3955,.T.);
#5572=ORIENTED_EDGE('',*,*,#3960,.T.);
#5573=ORIENTED_EDGE('',*,*,#3961,.F.);
#5574=ORIENTED_EDGE('',*,*,#3962,.T.);
#5575=ORIENTED_EDGE('',*,*,#3958,.T.);
#5576=ORIENTED_EDGE('',*,*,#3963,.T.);
#5577=ORIENTED_EDGE('',*,*,#3964,.F.);
#5578=ORIENTED_EDGE('',*,*,#3965,.T.);
#5579=ORIENTED_EDGE('',*,*,#3966,.F.);
#5580=ORIENTED_EDGE('',*,*,#3967,.F.);
#5581=ORIENTED_EDGE('',*,*,#3968,.F.);
#5582=ORIENTED_EDGE('',*,*,#3944,.F.);
#5583=ORIENTED_EDGE('',*,*,#3969,.F.);
#5584=ORIENTED_EDGE('',*,*,#3965,.F.);
#5585=ORIENTED_EDGE('',*,*,#3966,.T.);
#5586=ORIENTED_EDGE('',*,*,#3969,.T.);
#5587=ORIENTED_EDGE('',*,*,#3943,.F.);
#5588=ORIENTED_EDGE('',*,*,#3947,.F.);
#5589=ORIENTED_EDGE('',*,*,#3950,.F.);
#5590=ORIENTED_EDGE('',*,*,#3953,.F.);
#5591=ORIENTED_EDGE('',*,*,#3956,.F.);
#5592=ORIENTED_EDGE('',*,*,#3959,.F.);
#5593=ORIENTED_EDGE('',*,*,#3962,.F.);
#5594=ORIENTED_EDGE('',*,*,#3970,.F.);
#5595=ORIENTED_EDGE('',*,*,#3971,.F.);
#5596=ORIENTED_EDGE('',*,*,#3918,.F.);
#5597=ORIENTED_EDGE('',*,*,#3922,.F.);
#5598=ORIENTED_EDGE('',*,*,#3925,.F.);
#5599=ORIENTED_EDGE('',*,*,#3928,.F.);
#5600=ORIENTED_EDGE('',*,*,#3931,.F.);
#5601=ORIENTED_EDGE('',*,*,#3934,.F.);
#5602=ORIENTED_EDGE('',*,*,#3937,.F.);
#5603=ORIENTED_EDGE('',*,*,#3940,.F.);
#5604=ORIENTED_EDGE('',*,*,#3972,.F.);
#5605=ORIENTED_EDGE('',*,*,#3961,.T.);
#5606=ORIENTED_EDGE('',*,*,#3973,.T.);
#5607=ORIENTED_EDGE('',*,*,#3974,.F.);
#5608=ORIENTED_EDGE('',*,*,#3970,.T.);
#5609=ORIENTED_EDGE('',*,*,#3975,.F.);
#5610=ORIENTED_EDGE('',*,*,#3976,.T.);
#5611=ORIENTED_EDGE('',*,*,#3977,.T.);
#5612=ORIENTED_EDGE('',*,*,#3978,.F.);
#5613=ORIENTED_EDGE('',*,*,#3979,.F.);
#5614=ORIENTED_EDGE('',*,*,#3980,.T.);
#5615=ORIENTED_EDGE('',*,*,#3981,.T.);
#5616=ORIENTED_EDGE('',*,*,#3976,.F.);
#5617=ORIENTED_EDGE('',*,*,#3982,.F.);
#5618=ORIENTED_EDGE('',*,*,#3983,.T.);
#5619=ORIENTED_EDGE('',*,*,#3984,.T.);
#5620=ORIENTED_EDGE('',*,*,#3980,.F.);
#5621=ORIENTED_EDGE('',*,*,#3985,.F.);
#5622=ORIENTED_EDGE('',*,*,#3986,.T.);
#5623=ORIENTED_EDGE('',*,*,#3987,.T.);
#5624=ORIENTED_EDGE('',*,*,#3983,.F.);
#5625=ORIENTED_EDGE('',*,*,#3988,.F.);
#5626=ORIENTED_EDGE('',*,*,#3989,.T.);
#5627=ORIENTED_EDGE('',*,*,#3990,.T.);
#5628=ORIENTED_EDGE('',*,*,#3986,.F.);
#5629=ORIENTED_EDGE('',*,*,#3991,.F.);
#5630=ORIENTED_EDGE('',*,*,#3978,.T.);
#5631=ORIENTED_EDGE('',*,*,#3992,.T.);
#5632=ORIENTED_EDGE('',*,*,#3989,.F.);
#5633=ORIENTED_EDGE('',*,*,#3992,.F.);
#5634=ORIENTED_EDGE('',*,*,#3977,.F.);
#5635=ORIENTED_EDGE('',*,*,#3981,.F.);
#5636=ORIENTED_EDGE('',*,*,#3984,.F.);
#5637=ORIENTED_EDGE('',*,*,#3987,.F.);
#5638=ORIENTED_EDGE('',*,*,#3990,.F.);
#5639=ORIENTED_EDGE('',*,*,#3968,.T.);
#5640=ORIENTED_EDGE('',*,*,#3993,.T.);
#5641=ORIENTED_EDGE('',*,*,#3941,.T.);
#5642=ORIENTED_EDGE('',*,*,#3938,.T.);
#5643=ORIENTED_EDGE('',*,*,#3935,.T.);
#5644=ORIENTED_EDGE('',*,*,#3932,.T.);
#5645=ORIENTED_EDGE('',*,*,#3929,.T.);
#5646=ORIENTED_EDGE('',*,*,#3926,.T.);
#5647=ORIENTED_EDGE('',*,*,#3923,.T.);
#5648=ORIENTED_EDGE('',*,*,#3920,.T.);
#5649=ORIENTED_EDGE('',*,*,#3994,.F.);
#5650=ORIENTED_EDGE('',*,*,#3973,.F.);
#5651=ORIENTED_EDGE('',*,*,#3963,.F.);
#5652=ORIENTED_EDGE('',*,*,#3960,.F.);
#5653=ORIENTED_EDGE('',*,*,#3957,.F.);
#5654=ORIENTED_EDGE('',*,*,#3954,.F.);
#5655=ORIENTED_EDGE('',*,*,#3951,.F.);
#5656=ORIENTED_EDGE('',*,*,#3948,.F.);
#5657=ORIENTED_EDGE('',*,*,#3945,.F.);
#5658=ORIENTED_EDGE('',*,*,#3939,.T.);
#5659=ORIENTED_EDGE('',*,*,#3993,.F.);
#5660=ORIENTED_EDGE('',*,*,#3967,.T.);
#5661=ORIENTED_EDGE('',*,*,#3972,.T.);
#5662=ORIENTED_EDGE('',*,*,#3995,.F.);
#5663=ORIENTED_EDGE('',*,*,#3996,.T.);
#5664=ORIENTED_EDGE('',*,*,#3997,.F.);
#5665=ORIENTED_EDGE('',*,*,#3998,.T.);
#5666=ORIENTED_EDGE('',*,*,#3995,.T.);
#5667=ORIENTED_EDGE('',*,*,#3998,.F.);
#5668=ORIENTED_EDGE('',*,*,#3997,.T.);
#5669=ORIENTED_EDGE('',*,*,#3975,.T.);
#5670=ORIENTED_EDGE('',*,*,#3991,.T.);
#5671=ORIENTED_EDGE('',*,*,#3988,.T.);
#5672=ORIENTED_EDGE('',*,*,#3985,.T.);
#5673=ORIENTED_EDGE('',*,*,#3982,.T.);
#5674=ORIENTED_EDGE('',*,*,#3979,.T.);
#5675=ORIENTED_EDGE('',*,*,#3999,.F.);
#5676=ORIENTED_EDGE('',*,*,#3974,.T.);
#5677=ORIENTED_EDGE('',*,*,#3994,.T.);
#5678=ORIENTED_EDGE('',*,*,#3919,.T.);
#5679=ORIENTED_EDGE('',*,*,#3971,.T.);
#5680=ORIENTED_EDGE('',*,*,#3996,.F.);
#5681=ORIENTED_EDGE('',*,*,#4000,.T.);
#5682=ORIENTED_EDGE('',*,*,#3999,.T.);
#5683=ORIENTED_EDGE('',*,*,#4000,.F.);
#5684=ORIENTED_EDGE('',*,*,#3964,.T.);
#5685=ORIENTED_EDGE('',*,*,#4001,.F.);
#5686=ORIENTED_EDGE('',*,*,#4002,.T.);
#5687=ORIENTED_EDGE('',*,*,#4003,.T.);
#5688=ORIENTED_EDGE('',*,*,#4004,.T.);
#5689=ORIENTED_EDGE('',*,*,#4005,.F.);
#5690=ORIENTED_EDGE('',*,*,#4006,.T.);
#5691=ORIENTED_EDGE('',*,*,#4001,.T.);
#5692=ORIENTED_EDGE('',*,*,#4007,.T.);
#5693=ORIENTED_EDGE('',*,*,#4008,.F.);
#5694=ORIENTED_EDGE('',*,*,#4009,.T.);
#5695=ORIENTED_EDGE('',*,*,#4005,.T.);
#5696=ORIENTED_EDGE('',*,*,#4010,.T.);
#5697=ORIENTED_EDGE('',*,*,#4011,.F.);
#5698=ORIENTED_EDGE('',*,*,#4012,.T.);
#5699=ORIENTED_EDGE('',*,*,#4008,.T.);
#5700=ORIENTED_EDGE('',*,*,#4013,.T.);
#5701=ORIENTED_EDGE('',*,*,#4014,.F.);
#5702=ORIENTED_EDGE('',*,*,#4015,.T.);
#5703=ORIENTED_EDGE('',*,*,#4011,.T.);
#5704=ORIENTED_EDGE('',*,*,#4016,.T.);
#5705=ORIENTED_EDGE('',*,*,#4017,.F.);
#5706=ORIENTED_EDGE('',*,*,#4018,.T.);
#5707=ORIENTED_EDGE('',*,*,#4014,.T.);
#5708=ORIENTED_EDGE('',*,*,#4019,.T.);
#5709=ORIENTED_EDGE('',*,*,#4020,.F.);
#5710=ORIENTED_EDGE('',*,*,#4021,.T.);
#5711=ORIENTED_EDGE('',*,*,#4017,.T.);
#5712=ORIENTED_EDGE('',*,*,#4022,.T.);
#5713=ORIENTED_EDGE('',*,*,#4023,.F.);
#5714=ORIENTED_EDGE('',*,*,#4024,.T.);
#5715=ORIENTED_EDGE('',*,*,#4020,.T.);
#5716=ORIENTED_EDGE('',*,*,#4025,.T.);
#5717=ORIENTED_EDGE('',*,*,#4026,.F.);
#5718=ORIENTED_EDGE('',*,*,#4027,.T.);
#5719=ORIENTED_EDGE('',*,*,#4023,.T.);
#5720=ORIENTED_EDGE('',*,*,#4028,.T.);
#5721=ORIENTED_EDGE('',*,*,#4029,.F.);
#5722=ORIENTED_EDGE('',*,*,#4030,.T.);
#5723=ORIENTED_EDGE('',*,*,#4026,.T.);
#5724=ORIENTED_EDGE('',*,*,#4031,.T.);
#5725=ORIENTED_EDGE('',*,*,#4032,.F.);
#5726=ORIENTED_EDGE('',*,*,#4033,.T.);
#5727=ORIENTED_EDGE('',*,*,#4029,.T.);
#5728=ORIENTED_EDGE('',*,*,#4034,.T.);
#5729=ORIENTED_EDGE('',*,*,#4035,.F.);
#5730=ORIENTED_EDGE('',*,*,#4036,.T.);
#5731=ORIENTED_EDGE('',*,*,#4032,.T.);
#5732=ORIENTED_EDGE('',*,*,#4037,.T.);
#5733=ORIENTED_EDGE('',*,*,#4038,.F.);
#5734=ORIENTED_EDGE('',*,*,#4039,.T.);
#5735=ORIENTED_EDGE('',*,*,#4035,.T.);
#5736=ORIENTED_EDGE('',*,*,#4040,.T.);
#5737=ORIENTED_EDGE('',*,*,#4041,.F.);
#5738=ORIENTED_EDGE('',*,*,#4042,.T.);
#5739=ORIENTED_EDGE('',*,*,#4043,.T.);
#5740=ORIENTED_EDGE('',*,*,#4044,.F.);
#5741=ORIENTED_EDGE('',*,*,#4045,.F.);
#5742=ORIENTED_EDGE('',*,*,#4046,.T.);
#5743=ORIENTED_EDGE('',*,*,#4041,.T.);
#5744=ORIENTED_EDGE('',*,*,#4047,.F.);
#5745=ORIENTED_EDGE('',*,*,#4048,.F.);
#5746=ORIENTED_EDGE('',*,*,#4049,.T.);
#5747=ORIENTED_EDGE('',*,*,#4045,.T.);
#5748=ORIENTED_EDGE('',*,*,#4050,.F.);
#5749=ORIENTED_EDGE('',*,*,#4051,.F.);
#5750=ORIENTED_EDGE('',*,*,#4052,.T.);
#5751=ORIENTED_EDGE('',*,*,#4048,.T.);
#5752=ORIENTED_EDGE('',*,*,#4053,.F.);
#5753=ORIENTED_EDGE('',*,*,#4054,.F.);
#5754=ORIENTED_EDGE('',*,*,#4055,.T.);
#5755=ORIENTED_EDGE('',*,*,#4051,.T.);
#5756=ORIENTED_EDGE('',*,*,#4056,.F.);
#5757=ORIENTED_EDGE('',*,*,#4057,.F.);
#5758=ORIENTED_EDGE('',*,*,#4058,.T.);
#5759=ORIENTED_EDGE('',*,*,#4054,.T.);
#5760=ORIENTED_EDGE('',*,*,#4059,.F.);
#5761=ORIENTED_EDGE('',*,*,#4060,.F.);
#5762=ORIENTED_EDGE('',*,*,#4061,.T.);
#5763=ORIENTED_EDGE('',*,*,#4057,.T.);
#5764=ORIENTED_EDGE('',*,*,#4062,.F.);
#5765=ORIENTED_EDGE('',*,*,#4063,.F.);
#5766=ORIENTED_EDGE('',*,*,#4064,.T.);
#5767=ORIENTED_EDGE('',*,*,#4060,.T.);
#5768=ORIENTED_EDGE('',*,*,#4065,.F.);
#5769=ORIENTED_EDGE('',*,*,#4066,.F.);
#5770=ORIENTED_EDGE('',*,*,#4067,.T.);
#5771=ORIENTED_EDGE('',*,*,#4063,.T.);
#5772=ORIENTED_EDGE('',*,*,#4068,.F.);
#5773=ORIENTED_EDGE('',*,*,#4069,.F.);
#5774=ORIENTED_EDGE('',*,*,#4070,.T.);
#5775=ORIENTED_EDGE('',*,*,#4066,.T.);
#5776=ORIENTED_EDGE('',*,*,#4071,.F.);
#5777=ORIENTED_EDGE('',*,*,#4072,.F.);
#5778=ORIENTED_EDGE('',*,*,#4073,.T.);
#5779=ORIENTED_EDGE('',*,*,#4069,.T.);
#5780=ORIENTED_EDGE('',*,*,#4074,.F.);
#5781=ORIENTED_EDGE('',*,*,#4075,.F.);
#5782=ORIENTED_EDGE('',*,*,#4076,.T.);
#5783=ORIENTED_EDGE('',*,*,#4072,.T.);
#5784=ORIENTED_EDGE('',*,*,#4077,.F.);
#5785=ORIENTED_EDGE('',*,*,#4078,.F.);
#5786=ORIENTED_EDGE('',*,*,#4079,.T.);
#5787=ORIENTED_EDGE('',*,*,#4075,.T.);
#5788=ORIENTED_EDGE('',*,*,#4080,.F.);
#5789=ORIENTED_EDGE('',*,*,#4081,.F.);
#5790=ORIENTED_EDGE('',*,*,#4043,.F.);
#5791=ORIENTED_EDGE('',*,*,#4082,.F.);
#5792=ORIENTED_EDGE('',*,*,#4083,.F.);
#5793=ORIENTED_EDGE('',*,*,#4084,.F.);
#5794=ORIENTED_EDGE('',*,*,#4085,.T.);
#5795=ORIENTED_EDGE('',*,*,#4086,.F.);
#5796=ORIENTED_EDGE('',*,*,#4085,.F.);
#5797=ORIENTED_EDGE('',*,*,#4082,.T.);
#5798=ORIENTED_EDGE('',*,*,#4042,.F.);
#5799=ORIENTED_EDGE('',*,*,#4046,.F.);
#5800=ORIENTED_EDGE('',*,*,#4049,.F.);
#5801=ORIENTED_EDGE('',*,*,#4052,.F.);
#5802=ORIENTED_EDGE('',*,*,#4055,.F.);
#5803=ORIENTED_EDGE('',*,*,#4058,.F.);
#5804=ORIENTED_EDGE('',*,*,#4061,.F.);
#5805=ORIENTED_EDGE('',*,*,#4064,.F.);
#5806=ORIENTED_EDGE('',*,*,#4067,.F.);
#5807=ORIENTED_EDGE('',*,*,#4070,.F.);
#5808=ORIENTED_EDGE('',*,*,#4073,.F.);
#5809=ORIENTED_EDGE('',*,*,#4076,.F.);
#5810=ORIENTED_EDGE('',*,*,#4079,.F.);
#5811=ORIENTED_EDGE('',*,*,#4087,.F.);
#5812=ORIENTED_EDGE('',*,*,#4088,.F.);
#5813=ORIENTED_EDGE('',*,*,#4002,.F.);
#5814=ORIENTED_EDGE('',*,*,#4006,.F.);
#5815=ORIENTED_EDGE('',*,*,#4009,.F.);
#5816=ORIENTED_EDGE('',*,*,#4012,.F.);
#5817=ORIENTED_EDGE('',*,*,#4015,.F.);
#5818=ORIENTED_EDGE('',*,*,#4018,.F.);
#5819=ORIENTED_EDGE('',*,*,#4021,.F.);
#5820=ORIENTED_EDGE('',*,*,#4024,.F.);
#5821=ORIENTED_EDGE('',*,*,#4027,.F.);
#5822=ORIENTED_EDGE('',*,*,#4030,.F.);
#5823=ORIENTED_EDGE('',*,*,#4033,.F.);
#5824=ORIENTED_EDGE('',*,*,#4036,.F.);
#5825=ORIENTED_EDGE('',*,*,#4039,.F.);
#5826=ORIENTED_EDGE('',*,*,#4089,.F.);
#5827=ORIENTED_EDGE('',*,*,#4078,.T.);
#5828=ORIENTED_EDGE('',*,*,#4090,.F.);
#5829=ORIENTED_EDGE('',*,*,#4091,.F.);
#5830=ORIENTED_EDGE('',*,*,#4087,.T.);
#5831=ORIENTED_EDGE('',*,*,#4081,.T.);
#5832=ORIENTED_EDGE('',*,*,#4084,.T.);
#5833=ORIENTED_EDGE('',*,*,#4092,.F.);
#5834=ORIENTED_EDGE('',*,*,#4040,.F.);
#5835=ORIENTED_EDGE('',*,*,#4037,.F.);
#5836=ORIENTED_EDGE('',*,*,#4034,.F.);
#5837=ORIENTED_EDGE('',*,*,#4031,.F.);
#5838=ORIENTED_EDGE('',*,*,#4028,.F.);
#5839=ORIENTED_EDGE('',*,*,#4025,.F.);
#5840=ORIENTED_EDGE('',*,*,#4022,.F.);
#5841=ORIENTED_EDGE('',*,*,#4019,.F.);
#5842=ORIENTED_EDGE('',*,*,#4016,.F.);
#5843=ORIENTED_EDGE('',*,*,#4013,.F.);
#5844=ORIENTED_EDGE('',*,*,#4010,.F.);
#5845=ORIENTED_EDGE('',*,*,#4007,.F.);
#5846=ORIENTED_EDGE('',*,*,#4004,.F.);
#5847=ORIENTED_EDGE('',*,*,#4093,.F.);
#5848=ORIENTED_EDGE('',*,*,#4090,.T.);
#5849=ORIENTED_EDGE('',*,*,#4080,.T.);
#5850=ORIENTED_EDGE('',*,*,#4077,.T.);
#5851=ORIENTED_EDGE('',*,*,#4074,.T.);
#5852=ORIENTED_EDGE('',*,*,#4071,.T.);
#5853=ORIENTED_EDGE('',*,*,#4068,.T.);
#5854=ORIENTED_EDGE('',*,*,#4065,.T.);
#5855=ORIENTED_EDGE('',*,*,#4062,.T.);
#5856=ORIENTED_EDGE('',*,*,#4059,.T.);
#5857=ORIENTED_EDGE('',*,*,#4056,.T.);
#5858=ORIENTED_EDGE('',*,*,#4053,.T.);
#5859=ORIENTED_EDGE('',*,*,#4050,.T.);
#5860=ORIENTED_EDGE('',*,*,#4047,.T.);
#5861=ORIENTED_EDGE('',*,*,#4044,.T.);
#5862=ORIENTED_EDGE('',*,*,#4038,.T.);
#5863=ORIENTED_EDGE('',*,*,#4092,.T.);
#5864=ORIENTED_EDGE('',*,*,#4083,.T.);
#5865=ORIENTED_EDGE('',*,*,#4089,.T.);
#5866=ORIENTED_EDGE('',*,*,#4094,.F.);
#5867=ORIENTED_EDGE('',*,*,#4095,.T.);
#5868=ORIENTED_EDGE('',*,*,#4096,.T.);
#5869=ORIENTED_EDGE('',*,*,#4097,.F.);
#5870=ORIENTED_EDGE('',*,*,#4098,.F.);
#5871=ORIENTED_EDGE('',*,*,#4099,.T.);
#5872=ORIENTED_EDGE('',*,*,#4100,.T.);
#5873=ORIENTED_EDGE('',*,*,#4095,.F.);
#5874=ORIENTED_EDGE('',*,*,#4101,.F.);
#5875=ORIENTED_EDGE('',*,*,#4102,.T.);
#5876=ORIENTED_EDGE('',*,*,#4103,.T.);
#5877=ORIENTED_EDGE('',*,*,#4099,.F.);
#5878=ORIENTED_EDGE('',*,*,#4104,.F.);
#5879=ORIENTED_EDGE('',*,*,#4105,.T.);
#5880=ORIENTED_EDGE('',*,*,#4106,.T.);
#5881=ORIENTED_EDGE('',*,*,#4102,.F.);
#5882=ORIENTED_EDGE('',*,*,#4107,.F.);
#5883=ORIENTED_EDGE('',*,*,#4108,.T.);
#5884=ORIENTED_EDGE('',*,*,#4109,.T.);
#5885=ORIENTED_EDGE('',*,*,#4105,.F.);
#5886=ORIENTED_EDGE('',*,*,#4110,.F.);
#5887=ORIENTED_EDGE('',*,*,#4097,.T.);
#5888=ORIENTED_EDGE('',*,*,#4111,.T.);
#5889=ORIENTED_EDGE('',*,*,#4108,.F.);
#5890=ORIENTED_EDGE('',*,*,#4111,.F.);
#5891=ORIENTED_EDGE('',*,*,#4096,.F.);
#5892=ORIENTED_EDGE('',*,*,#4100,.F.);
#5893=ORIENTED_EDGE('',*,*,#4103,.F.);
#5894=ORIENTED_EDGE('',*,*,#4106,.F.);
#5895=ORIENTED_EDGE('',*,*,#4109,.F.);
#5896=ORIENTED_EDGE('',*,*,#4112,.T.);
#5897=ORIENTED_EDGE('',*,*,#4088,.T.);
#5898=ORIENTED_EDGE('',*,*,#4091,.T.);
#5899=ORIENTED_EDGE('',*,*,#4093,.T.);
#5900=ORIENTED_EDGE('',*,*,#4003,.F.);
#5901=ORIENTED_EDGE('',*,*,#4112,.F.);
#5902=ORIENTED_EDGE('',*,*,#4113,.T.);
#5903=ORIENTED_EDGE('',*,*,#4114,.T.);
#5904=ORIENTED_EDGE('',*,*,#4113,.F.);
#5905=ORIENTED_EDGE('',*,*,#4114,.F.);
#5906=ORIENTED_EDGE('',*,*,#4094,.T.);
#5907=ORIENTED_EDGE('',*,*,#4110,.T.);
#5908=ORIENTED_EDGE('',*,*,#4107,.T.);
#5909=ORIENTED_EDGE('',*,*,#4104,.T.);
#5910=ORIENTED_EDGE('',*,*,#4101,.T.);
#5911=ORIENTED_EDGE('',*,*,#4098,.T.);
#5912=ORIENTED_EDGE('',*,*,#4086,.T.);
#5913=PLANE('',#6655);
#5914=PLANE('',#6662);
#5915=PLANE('',#6681);
#5916=PLANE('',#6682);
#5917=PLANE('',#6683);
#5918=PLANE('',#6684);
#5919=PLANE('',#6685);
#5920=PLANE('',#6686);
#5921=PLANE('',#6687);
#5922=PLANE('',#6688);
#5923=PLANE('',#6689);
#5924=PLANE('',#6690);
#5925=PLANE('',#6691);
#5926=PLANE('',#6692);
#5927=PLANE('',#6693);
#5928=PLANE('',#6694);
#5929=PLANE('',#6695);
#5930=PLANE('',#6696);
#5931=PLANE('',#6697);
#5932=PLANE('',#6698);
#5933=PLANE('',#6699);
#5934=PLANE('',#6700);
#5935=PLANE('',#6701);
#5936=PLANE('',#6702);
#5937=PLANE('',#6776);
#5938=PLANE('',#6779);
#5939=PLANE('',#6782);
#5940=PLANE('',#6783);
#5941=PLANE('',#6793);
#5942=PLANE('',#6794);
#5943=PLANE('',#6795);
#5944=PLANE('',#6796);
#5945=PLANE('',#6797);
#5946=PLANE('',#6798);
#5947=PLANE('',#6799);
#5948=PLANE('',#6800);
#5949=PLANE('',#6801);
#5950=PLANE('',#6802);
#5951=PLANE('',#6803);
#5952=PLANE('',#6804);
#5953=PLANE('',#6805);
#5954=PLANE('',#6806);
#5955=PLANE('',#6807);
#5956=PLANE('',#6808);
#5957=PLANE('',#6809);
#5958=PLANE('',#6810);
#5959=PLANE('',#6811);
#5960=PLANE('',#6812);
#5961=PLANE('',#6813);
#5962=PLANE('',#6814);
#5963=PLANE('',#6815);
#5964=PLANE('',#6816);
#5965=PLANE('',#6817);
#5966=PLANE('',#6818);
#5967=PLANE('',#6819);
#5968=PLANE('',#6820);
#5969=PLANE('',#6821);
#5970=PLANE('',#6822);
#5971=PLANE('',#6823);
#5972=PLANE('',#6824);
#5973=PLANE('',#6825);
#5974=PLANE('',#6826);
#5975=PLANE('',#6865);
#5976=PLANE('',#6882);
#5977=PLANE('',#6886);
#5978=PLANE('',#6887);
#5979=PLANE('',#6888);
#5980=PLANE('',#6889);
#5981=PLANE('',#6894);
#5982=PLANE('',#6895);
#5983=PLANE('',#6897);
#5984=PLANE('',#6900);
#5985=PLANE('',#6904);
#5986=PLANE('',#6908);
#5987=PLANE('',#6909);
#5988=PLANE('',#6910);
#5989=PLANE('',#6911);
#5990=PLANE('',#6912);
#5991=PLANE('',#6913);
#5992=PLANE('',#6914);
#5993=PLANE('',#6915);
#5994=PLANE('',#6916);
#5995=PLANE('',#6917);
#5996=PLANE('',#6918);
#5997=PLANE('',#6919);
#5998=PLANE('',#6920);
#5999=PLANE('',#6921);
#6000=PLANE('',#6922);
#6001=PLANE('',#6923);
#6002=PLANE('',#6924);
#6003=PLANE('',#6925);
#6004=PLANE('',#6930);
#6005=PLANE('',#6932);
#6006=PLANE('',#6936);
#6007=PLANE('',#6941);
#6008=PLANE('',#6943);
#6009=PLANE('',#6948);
#6010=PLANE('',#6950);
#6011=PLANE('',#6954);
#6012=PLANE('',#6959);
#6013=PLANE('',#6961);
#6014=PLANE('',#6969);
#6015=PLANE('',#6970);
#6016=PLANE('',#6972);
#6017=PLANE('',#6973);
#6018=PLANE('',#6974);
#6019=PLANE('',#6981);
#6020=PLANE('',#6989);
#6021=PLANE('',#6990);
#6022=PLANE('',#6998);
#6023=PLANE('',#6999);
#6024=PLANE('',#7007);
#6025=PLANE('',#7008);
#6026=PLANE('',#7010);
#6027=PLANE('',#7011);
#6028=PLANE('',#7012);
#6029=PLANE('',#7019);
#6030=PLANE('',#7024);
#6031=PLANE('',#7026);
#6032=PLANE('',#7030);
#6033=PLANE('',#7035);
#6034=PLANE('',#7037);
#6035=PLANE('',#7045);
#6036=PLANE('',#7046);
#6037=PLANE('',#7054);
#6038=PLANE('',#7055);
#6039=PLANE('',#7057);
#6040=PLANE('',#7058);
#6041=PLANE('',#7059);
#6042=PLANE('',#7066);
#6043=PLANE('',#7074);
#6044=PLANE('',#7075);
#6045=PLANE('',#7099);
#6046=PLANE('',#7100);
#6047=PLANE('',#7101);
#6048=PLANE('',#7102);
#6049=PLANE('',#7103);
#6050=PLANE('',#7104);
#6051=PLANE('',#7105);
#6052=PLANE('',#7107);
#6053=PLANE('',#7112);
#6054=PLANE('',#7113);
#6055=PLANE('',#7116);
#6056=PLANE('',#7152);
#6057=PLANE('',#7153);
#6058=PLANE('',#7154);
#6059=PLANE('',#7155);
#6060=PLANE('',#7156);
#6061=PLANE('',#7157);
#6062=PLANE('',#7158);
#6063=PLANE('',#7159);
#6064=PLANE('',#7163);
#6065=PLANE('',#7164);
#6066=ADVANCED_FACE('',(#1687,#1616),#5913,.F.);
#6067=ADVANCED_FACE('',(#1688),#1423,.F.);
#6068=ADVANCED_FACE('',(#1689),#1424,.F.);
#6069=ADVANCED_FACE('',(#1690,#1617),#5914,.F.);
#6070=ADVANCED_FACE('',(#1691),#1425,.F.);
#6071=ADVANCED_FACE('',(#1692),#1426,.F.);
#6072=ADVANCED_FACE('',(#1693),#1427,.F.);
#6073=ADVANCED_FACE('',(#1694),#1428,.F.);
#6074=ADVANCED_FACE('',(#1695),#1429,.F.);
#6075=ADVANCED_FACE('',(#1696),#1430,.F.);
#6076=ADVANCED_FACE('',(#1697),#5915,.F.);
#6077=ADVANCED_FACE('',(#1698),#5916,.F.);
#6078=ADVANCED_FACE('',(#1699),#5917,.F.);
#6079=ADVANCED_FACE('',(#1700),#5918,.F.);
#6080=ADVANCED_FACE('',(#1701),#5919,.F.);
#6081=ADVANCED_FACE('',(#1702),#5920,.F.);
#6082=ADVANCED_FACE('',(#1703),#5921,.F.);
#6083=ADVANCED_FACE('',(#1704),#5922,.F.);
#6084=ADVANCED_FACE('',(#1705),#5923,.T.);
#6085=ADVANCED_FACE('',(#1706),#5924,.T.);
#6086=ADVANCED_FACE('',(#1707),#5925,.T.);
#6087=ADVANCED_FACE('',(#1708,#1618,#1619,#1620),#5926,.T.);
#6088=ADVANCED_FACE('',(#1709,#1621,#1622),#5927,.T.);
#6089=ADVANCED_FACE('',(#1710),#5928,.T.);
#6090=ADVANCED_FACE('',(#1711),#5929,.T.);
#6091=ADVANCED_FACE('',(#1712),#5930,.T.);
#6092=ADVANCED_FACE('',(#1713,#1623,#1624,#1625),#5931,.T.);
#6093=ADVANCED_FACE('',(#1714),#5932,.T.);
#6094=ADVANCED_FACE('',(#1715),#5933,.T.);
#6095=ADVANCED_FACE('',(#1716),#5934,.T.);
#6096=ADVANCED_FACE('',(#1717),#5935,.T.);
#6097=ADVANCED_FACE('',(#1718,#1626,#1627,#1628,#1629,#1630,#1631,#1632,
#1633),#5936,.F.);
#6098=ADVANCED_FACE('',(#1719),#1431,.F.);
#6099=ADVANCED_FACE('',(#1720),#1432,.F.);
#6100=ADVANCED_FACE('',(#1721),#1433,.F.);
#6101=ADVANCED_FACE('',(#1722),#1434,.F.);
#6102=ADVANCED_FACE('',(#1723),#1435,.F.);
#6103=ADVANCED_FACE('',(#1724),#1436,.F.);
#6104=ADVANCED_FACE('',(#1725),#1437,.F.);
#6105=ADVANCED_FACE('',(#1726),#1438,.F.);
#6106=ADVANCED_FACE('',(#1727),#1439,.F.);
#6107=ADVANCED_FACE('',(#1728),#1440,.F.);
#6108=ADVANCED_FACE('',(#1729),#1441,.F.);
#6109=ADVANCED_FACE('',(#1730),#1442,.F.);
#6110=ADVANCED_FACE('',(#1731),#1443,.F.);
#6111=ADVANCED_FACE('',(#1732),#1444,.F.);
#6112=ADVANCED_FACE('',(#1733),#1445,.F.);
#6113=ADVANCED_FACE('',(#1734),#1446,.F.);
#6114=ADVANCED_FACE('',(#1735),#1447,.F.);
#6115=ADVANCED_FACE('',(#1736),#1448,.F.);
#6116=ADVANCED_FACE('',(#1737),#1449,.F.);
#6117=ADVANCED_FACE('',(#1738),#1450,.F.);
#6118=ADVANCED_FACE('',(#1739),#1451,.F.);
#6119=ADVANCED_FACE('',(#1740),#1452,.F.);
#6120=ADVANCED_FACE('',(#1741),#1453,.F.);
#6121=ADVANCED_FACE('',(#1742),#1454,.F.);
#6122=ADVANCED_FACE('',(#1743),#1455,.F.);
#6123=ADVANCED_FACE('',(#1744),#1456,.F.);
#6124=ADVANCED_FACE('',(#1745),#1457,.F.);
#6125=ADVANCED_FACE('',(#1746),#1458,.F.);
#6126=ADVANCED_FACE('',(#1747),#1459,.F.);
#6127=ADVANCED_FACE('',(#1748),#1460,.F.);
#6128=ADVANCED_FACE('',(#1749),#1461,.F.);
#6129=ADVANCED_FACE('',(#1750),#1462,.F.);
#6130=ADVANCED_FACE('',(#1751),#1463,.F.);
#6131=ADVANCED_FACE('',(#1752),#1464,.F.);
#6132=ADVANCED_FACE('',(#1753),#1465,.F.);
#6133=ADVANCED_FACE('',(#1754),#1466,.F.);
#6134=ADVANCED_FACE('',(#1755),#1467,.F.);
#6135=ADVANCED_FACE('',(#1756),#1468,.F.);
#6136=ADVANCED_FACE('',(#1757),#1469,.F.);
#6137=ADVANCED_FACE('',(#1758),#1470,.F.);
#6138=ADVANCED_FACE('',(#1759),#1471,.F.);
#6139=ADVANCED_FACE('',(#1760),#1472,.F.);
#6140=ADVANCED_FACE('',(#1761),#1473,.F.);
#6141=ADVANCED_FACE('',(#1762),#1474,.F.);
#6142=ADVANCED_FACE('',(#1763),#1475,.F.);
#6143=ADVANCED_FACE('',(#1764),#1476,.F.);
#6144=ADVANCED_FACE('',(#1765),#1477,.F.);
#6145=ADVANCED_FACE('',(#1766),#1478,.F.);
#6146=ADVANCED_FACE('',(#1767),#1479,.F.);
#6147=ADVANCED_FACE('',(#1768),#1480,.F.);
#6148=ADVANCED_FACE('',(#1769),#1481,.F.);
#6149=ADVANCED_FACE('',(#1770),#1482,.F.);
#6150=ADVANCED_FACE('',(#1771),#1483,.F.);
#6151=ADVANCED_FACE('',(#1772),#1484,.F.);
#6152=ADVANCED_FACE('',(#1773),#1485,.F.);
#6153=ADVANCED_FACE('',(#1774),#1486,.F.);
#6154=ADVANCED_FACE('',(#1775),#1487,.F.);
#6155=ADVANCED_FACE('',(#1776),#1488,.F.);
#6156=ADVANCED_FACE('',(#1777),#1489,.F.);
#6157=ADVANCED_FACE('',(#1778),#1490,.F.);
#6158=ADVANCED_FACE('',(#1779),#1491,.F.);
#6159=ADVANCED_FACE('',(#1780),#1492,.F.);
#6160=ADVANCED_FACE('',(#1781),#5937,.T.);
#6161=ADVANCED_FACE('',(#1782),#1493,.F.);
#6162=ADVANCED_FACE('',(#1783),#117,.F.);
#6163=ADVANCED_FACE('',(#1784),#118,.F.);
#6164=ADVANCED_FACE('',(#1785),#1494,.F.);
#6165=ADVANCED_FACE('',(#1786),#5938,.T.);
#6166=ADVANCED_FACE('',(#1787),#1495,.F.);
#6167=ADVANCED_FACE('',(#1788),#119,.F.);
#6168=ADVANCED_FACE('',(#1789),#120,.F.);
#6169=ADVANCED_FACE('',(#1790),#1496,.F.);
#6170=ADVANCED_FACE('',(#1791),#5939,.F.);
#6171=ADVANCED_FACE('',(#1792),#5940,.F.);
#6172=ADVANCED_FACE('',(#1793),#1497,.F.);
#6173=ADVANCED_FACE('',(#1794),#1498,.F.);
#6174=ADVANCED_FACE('',(#1795),#1499,.F.);
#6175=ADVANCED_FACE('',(#1796),#5941,.T.);
#6176=ADVANCED_FACE('',(#1797),#5942,.T.);
#6177=ADVANCED_FACE('',(#1798),#5943,.F.);
#6178=ADVANCED_FACE('',(#1799),#5944,.F.);
#6179=ADVANCED_FACE('',(#1800),#5945,.F.);
#6180=ADVANCED_FACE('',(#1801,#1634),#5946,.T.);
#6181=ADVANCED_FACE('',(#1802),#5947,.T.);
#6182=ADVANCED_FACE('',(#1803),#5948,.T.);
#6183=ADVANCED_FACE('',(#1804),#5949,.F.);
#6184=ADVANCED_FACE('',(#1805,#1635,#1636),#5950,.F.);
#6185=ADVANCED_FACE('',(#1806,#1637,#1638),#5951,.T.);
#6186=ADVANCED_FACE('',(#1807),#5952,.T.);
#6187=ADVANCED_FACE('',(#1808),#5953,.T.);
#6188=ADVANCED_FACE('',(#1809,#1639,#1640),#5954,.T.);
#6189=ADVANCED_FACE('',(#1810),#5955,.F.);
#6190=ADVANCED_FACE('',(#1811),#5956,.F.);
#6191=ADVANCED_FACE('',(#1812),#5957,.F.);
#6192=ADVANCED_FACE('',(#1813),#5958,.F.);
#6193=ADVANCED_FACE('',(#1814),#5959,.F.);
#6194=ADVANCED_FACE('',(#1815),#5960,.F.);
#6195=ADVANCED_FACE('',(#1816),#5961,.F.);
#6196=ADVANCED_FACE('',(#1817),#5962,.F.);
#6197=ADVANCED_FACE('',(#1818),#5963,.T.);
#6198=ADVANCED_FACE('',(#1819),#5964,.F.);
#6199=ADVANCED_FACE('',(#1820),#5965,.F.);
#6200=ADVANCED_FACE('',(#1821),#5966,.T.);
#6201=ADVANCED_FACE('',(#1822),#5967,.T.);
#6202=ADVANCED_FACE('',(#1823),#5968,.T.);
#6203=ADVANCED_FACE('',(#1824,#1641,#1642),#5969,.T.);
#6204=ADVANCED_FACE('',(#1825,#1643),#5970,.T.);
#6205=ADVANCED_FACE('',(#1826,#1644),#5971,.T.);
#6206=ADVANCED_FACE('',(#1827,#1645),#5972,.T.);
#6207=ADVANCED_FACE('',(#1828),#5973,.T.);
#6208=ADVANCED_FACE('',(#1829),#5974,.T.);
#6209=ADVANCED_FACE('',(#1830),#1500,.F.);
#6210=ADVANCED_FACE('',(#1831),#1501,.F.);
#6211=ADVANCED_FACE('',(#1832),#1502,.F.);
#6212=ADVANCED_FACE('',(#1833),#1503,.F.);
#6213=ADVANCED_FACE('',(#1834),#1504,.F.);
#6214=ADVANCED_FACE('',(#1835),#1505,.F.);
#6215=ADVANCED_FACE('',(#1836),#1506,.F.);
#6216=ADVANCED_FACE('',(#1837),#1507,.F.);
#6217=ADVANCED_FACE('',(#1838),#1508,.F.);
#6218=ADVANCED_FACE('',(#1839),#1509,.F.);
#6219=ADVANCED_FACE('',(#1840),#1510,.F.);
#6220=ADVANCED_FACE('',(#1841),#1511,.F.);
#6221=ADVANCED_FACE('',(#1842),#1512,.F.);
#6222=ADVANCED_FACE('',(#1843),#1513,.F.);
#6223=ADVANCED_FACE('',(#1844),#1514,.F.);
#6224=ADVANCED_FACE('',(#1845),#1515,.F.);
#6225=ADVANCED_FACE('',(#1846),#1516,.F.);
#6226=ADVANCED_FACE('',(#1847),#1517,.F.);
#6227=ADVANCED_FACE('',(#1848),#1518,.F.);
#6228=ADVANCED_FACE('',(#1849),#1519,.F.);
#6229=ADVANCED_FACE('',(#1850),#1520,.F.);
#6230=ADVANCED_FACE('',(#1851),#1521,.F.);
#6231=ADVANCED_FACE('',(#1852),#1522,.T.);
#6232=ADVANCED_FACE('',(#1853),#1523,.F.);
#6233=ADVANCED_FACE('',(#1854),#1524,.F.);
#6234=ADVANCED_FACE('',(#1855),#121,.F.);
#6235=ADVANCED_FACE('',(#1856),#122,.F.);
#6236=ADVANCED_FACE('',(#1857,#1646),#5975,.T.);
#6237=ADVANCED_FACE('',(#1858),#1525,.F.);
#6238=ADVANCED_FACE('',(#1859),#1526,.F.);
#6239=ADVANCED_FACE('',(#1860),#1527,.F.);
#6240=ADVANCED_FACE('',(#1861),#1528,.F.);
#6241=ADVANCED_FACE('',(#1862),#1529,.T.);
#6242=ADVANCED_FACE('',(#1863),#1530,.T.);
#6243=ADVANCED_FACE('',(#1864,#1647,#1648,#1649,#1650,#1651),#5976,.T.);
#6244=ADVANCED_FACE('',(#1865),#5977,.T.);
#6245=ADVANCED_FACE('',(#1866),#5978,.T.);
#6246=ADVANCED_FACE('',(#1867),#5979,.T.);
#6247=ADVANCED_FACE('',(#1868,#1652,#1653,#1654,#1655,#1656),#5980,.F.);
#6248=ADVANCED_FACE('',(#1869),#1531,.T.);
#6249=ADVANCED_FACE('',(#1870),#5981,.T.);
#6250=ADVANCED_FACE('',(#1871),#5982,.T.);
#6251=ADVANCED_FACE('',(#1872),#1532,.T.);
#6252=ADVANCED_FACE('',(#1873),#5983,.T.);
#6253=ADVANCED_FACE('',(#1874),#1533,.T.);
#6254=ADVANCED_FACE('',(#1875),#5984,.F.);
#6255=ADVANCED_FACE('',(#1876),#1534,.F.);
#6256=ADVANCED_FACE('',(#1877),#5985,.F.);
#6257=ADVANCED_FACE('',(#1878),#1535,.F.);
#6258=ADVANCED_FACE('',(#1879),#5986,.F.);
#6259=ADVANCED_FACE('',(#1880),#5987,.F.);
#6260=ADVANCED_FACE('',(#1881),#5988,.T.);
#6261=ADVANCED_FACE('',(#1882),#5989,.T.);
#6262=ADVANCED_FACE('',(#1883),#5990,.T.);
#6263=ADVANCED_FACE('',(#1884),#5991,.T.);
#6264=ADVANCED_FACE('',(#1885),#5992,.T.);
#6265=ADVANCED_FACE('',(#1886),#5993,.T.);
#6266=ADVANCED_FACE('',(#1887),#5994,.T.);
#6267=ADVANCED_FACE('',(#1888),#5995,.T.);
#6268=ADVANCED_FACE('',(#1889),#5996,.T.);
#6269=ADVANCED_FACE('',(#1890),#5997,.T.);
#6270=ADVANCED_FACE('',(#1891,#1657),#5998,.T.);
#6271=ADVANCED_FACE('',(#1892),#5999,.T.);
#6272=ADVANCED_FACE('',(#1893,#1658),#6000,.T.);
#6273=ADVANCED_FACE('',(#1894),#6001,.T.);
#6274=ADVANCED_FACE('',(#1895),#6002,.T.);
#6275=ADVANCED_FACE('',(#1896),#6003,.F.);
#6276=ADVANCED_FACE('',(#1897),#1536,.T.);
#6277=ADVANCED_FACE('',(#1898,#1659),#6004,.F.);
#6278=ADVANCED_FACE('',(#1899,#1660),#6005,.F.);
#6279=ADVANCED_FACE('',(#1900),#1537,.T.);
#6280=ADVANCED_FACE('',(#1901,#1661),#6006,.T.);
#6281=ADVANCED_FACE('',(#1902),#1538,.T.);
#6282=ADVANCED_FACE('',(#1903),#6007,.F.);
#6283=ADVANCED_FACE('',(#1904),#1539,.T.);
#6284=ADVANCED_FACE('',(#1905),#6008,.T.);
#6285=ADVANCED_FACE('',(#1906),#1540,.T.);
#6286=ADVANCED_FACE('',(#1907,#1662),#6009,.F.);
#6287=ADVANCED_FACE('',(#1908,#1663),#6010,.F.);
#6288=ADVANCED_FACE('',(#1909),#1541,.T.);
#6289=ADVANCED_FACE('',(#1910,#1664),#6011,.T.);
#6290=ADVANCED_FACE('',(#1911),#1542,.T.);
#6291=ADVANCED_FACE('',(#1912),#6012,.F.);
#6292=ADVANCED_FACE('',(#1913),#1543,.T.);
#6293=ADVANCED_FACE('',(#1914),#6013,.T.);
#6294=ADVANCED_FACE('',(#1915),#1544,.F.);
#6295=ADVANCED_FACE('',(#1916),#1545,.T.);
#6296=ADVANCED_FACE('',(#1917,#1665),#6014,.T.);
#6297=ADVANCED_FACE('',(#1918,#1666),#6015,.F.);
#6298=ADVANCED_FACE('',(#1919),#6016,.F.);
#6299=ADVANCED_FACE('',(#1920),#6017,.F.);
#6300=ADVANCED_FACE('',(#1921),#6018,.F.);
#6301=ADVANCED_FACE('',(#1922),#1546,.F.);
#6302=ADVANCED_FACE('',(#1923),#1547,.T.);
#6303=ADVANCED_FACE('',(#1924),#6019,.T.);
#6304=ADVANCED_FACE('',(#1925),#1548,.F.);
#6305=ADVANCED_FACE('',(#1926),#1549,.T.);
#6306=ADVANCED_FACE('',(#1927,#1667),#6020,.T.);
#6307=ADVANCED_FACE('',(#1928,#1668),#6021,.F.);
#6308=ADVANCED_FACE('',(#1929),#1550,.F.);
#6309=ADVANCED_FACE('',(#1930),#1551,.T.);
#6310=ADVANCED_FACE('',(#1931,#1669),#6022,.T.);
#6311=ADVANCED_FACE('',(#1932,#1670),#6023,.F.);
#6312=ADVANCED_FACE('',(#1933),#1552,.F.);
#6313=ADVANCED_FACE('',(#1934),#1553,.T.);
#6314=ADVANCED_FACE('',(#1935,#1671),#6024,.T.);
#6315=ADVANCED_FACE('',(#1936,#1672),#6025,.F.);
#6316=ADVANCED_FACE('',(#1937),#6026,.F.);
#6317=ADVANCED_FACE('',(#1938),#6027,.F.);
#6318=ADVANCED_FACE('',(#1939),#6028,.F.);
#6319=ADVANCED_FACE('',(#1940),#1554,.F.);
#6320=ADVANCED_FACE('',(#1941),#1555,.T.);
#6321=ADVANCED_FACE('',(#1942),#6029,.T.);
#6322=ADVANCED_FACE('',(#1943),#1556,.T.);
#6323=ADVANCED_FACE('',(#1944,#1673),#6030,.F.);
#6324=ADVANCED_FACE('',(#1945,#1674),#6031,.F.);
#6325=ADVANCED_FACE('',(#1946),#1557,.T.);
#6326=ADVANCED_FACE('',(#1947,#1675),#6032,.T.);
#6327=ADVANCED_FACE('',(#1948),#1558,.T.);
#6328=ADVANCED_FACE('',(#1949),#6033,.F.);
#6329=ADVANCED_FACE('',(#1950),#1559,.T.);
#6330=ADVANCED_FACE('',(#1951),#6034,.T.);
#6331=ADVANCED_FACE('',(#1952),#1560,.F.);
#6332=ADVANCED_FACE('',(#1953),#1561,.T.);
#6333=ADVANCED_FACE('',(#1954,#1676),#6035,.T.);
#6334=ADVANCED_FACE('',(#1955,#1677),#6036,.F.);
#6335=ADVANCED_FACE('',(#1956),#1562,.F.);
#6336=ADVANCED_FACE('',(#1957),#1563,.T.);
#6337=ADVANCED_FACE('',(#1958,#1678),#6037,.T.);
#6338=ADVANCED_FACE('',(#1959,#1679),#6038,.F.);
#6339=ADVANCED_FACE('',(#1960),#6039,.F.);
#6340=ADVANCED_FACE('',(#1961),#6040,.F.);
#6341=ADVANCED_FACE('',(#1962),#6041,.F.);
#6342=ADVANCED_FACE('',(#1963),#1564,.F.);
#6343=ADVANCED_FACE('',(#1964),#1565,.T.);
#6344=ADVANCED_FACE('',(#1965),#6042,.T.);
#6345=ADVANCED_FACE('',(#1966),#1566,.F.);
#6346=ADVANCED_FACE('',(#1967),#1567,.T.);
#6347=ADVANCED_FACE('',(#1968,#1680),#6043,.T.);
#6348=ADVANCED_FACE('',(#1969,#1681),#6044,.F.);
#6349=ADVANCED_FACE('',(#1970),#1568,.T.);
#6350=ADVANCED_FACE('',(#1971),#1569,.T.);
#6351=ADVANCED_FACE('',(#1972),#1570,.T.);
#6352=ADVANCED_FACE('',(#1973),#1571,.T.);
#6353=ADVANCED_FACE('',(#1974),#1572,.T.);
#6354=ADVANCED_FACE('',(#1975),#1573,.T.);
#6355=ADVANCED_FACE('',(#1976),#1574,.T.);
#6356=ADVANCED_FACE('',(#1977),#1575,.T.);
#6357=ADVANCED_FACE('',(#1978),#1576,.T.);
#6358=ADVANCED_FACE('',(#1979),#1577,.T.);
#6359=ADVANCED_FACE('',(#1980),#1578,.T.);
#6360=ADVANCED_FACE('',(#1981),#1579,.T.);
#6361=ADVANCED_FACE('',(#1982),#1580,.T.);
#6362=ADVANCED_FACE('',(#1983),#1581,.T.);
#6363=ADVANCED_FACE('',(#1984),#1582,.T.);
#6364=ADVANCED_FACE('',(#1985),#115,.T.);
#6365=ADVANCED_FACE('',(#1986),#123,.F.);
#6366=ADVANCED_FACE('',(#1987),#1583,.T.);
#6367=ADVANCED_FACE('',(#1988),#6045,.F.);
#6368=ADVANCED_FACE('',(#1989),#6046,.F.);
#6369=ADVANCED_FACE('',(#1990),#6047,.F.);
#6370=ADVANCED_FACE('',(#1991),#6048,.F.);
#6371=ADVANCED_FACE('',(#1992),#6049,.F.);
#6372=ADVANCED_FACE('',(#1993),#6050,.F.);
#6373=ADVANCED_FACE('',(#1994),#6051,.F.);
#6374=ADVANCED_FACE('',(#1995),#124,.F.);
#6375=ADVANCED_FACE('',(#1996),#1584,.T.);
#6376=ADVANCED_FACE('',(#1997,#1682),#6052,.F.);
#6377=ADVANCED_FACE('',(#1998),#1585,.T.);
#6378=ADVANCED_FACE('',(#1999,#1683),#6053,.T.);
#6379=ADVANCED_FACE('',(#2000,#1684),#6054,.F.);
#6380=ADVANCED_FACE('',(#2001),#1586,.T.);
#6381=ADVANCED_FACE('',(#2002),#6055,.F.);
#6382=ADVANCED_FACE('',(#2003),#1587,.T.);
#6383=ADVANCED_FACE('',(#2004),#1588,.T.);
#6384=ADVANCED_FACE('',(#2005),#1589,.T.);
#6385=ADVANCED_FACE('',(#2006),#1590,.T.);
#6386=ADVANCED_FACE('',(#2007),#1591,.T.);
#6387=ADVANCED_FACE('',(#2008),#1592,.T.);
#6388=ADVANCED_FACE('',(#2009),#1593,.T.);
#6389=ADVANCED_FACE('',(#2010),#1594,.T.);
#6390=ADVANCED_FACE('',(#2011),#1595,.T.);
#6391=ADVANCED_FACE('',(#2012),#1596,.T.);
#6392=ADVANCED_FACE('',(#2013),#1597,.T.);
#6393=ADVANCED_FACE('',(#2014),#1598,.T.);
#6394=ADVANCED_FACE('',(#2015),#1599,.T.);
#6395=ADVANCED_FACE('',(#2016),#1600,.T.);
#6396=ADVANCED_FACE('',(#2017),#1601,.T.);
#6397=ADVANCED_FACE('',(#2018),#1602,.T.);
#6398=ADVANCED_FACE('',(#2019),#1603,.T.);
#6399=ADVANCED_FACE('',(#2020),#1604,.T.);
#6400=ADVANCED_FACE('',(#2021),#1605,.T.);
#6401=ADVANCED_FACE('',(#2022),#1606,.T.);
#6402=ADVANCED_FACE('',(#2023),#1607,.T.);
#6403=ADVANCED_FACE('',(#2024),#1608,.T.);
#6404=ADVANCED_FACE('',(#2025),#1609,.T.);
#6405=ADVANCED_FACE('',(#2026),#1610,.T.);
#6406=ADVANCED_FACE('',(#2027),#1611,.T.);
#6407=ADVANCED_FACE('',(#2028),#1612,.T.);
#6408=ADVANCED_FACE('',(#2029),#116,.T.);
#6409=ADVANCED_FACE('',(#2030),#125,.F.);
#6410=ADVANCED_FACE('',(#2031),#1613,.T.);
#6411=ADVANCED_FACE('',(#2032),#126,.F.);
#6412=ADVANCED_FACE('',(#2033),#1614,.T.);
#6413=ADVANCED_FACE('',(#2034),#6056,.F.);
#6414=ADVANCED_FACE('',(#2035),#6057,.F.);
#6415=ADVANCED_FACE('',(#2036),#6058,.F.);
#6416=ADVANCED_FACE('',(#2037),#6059,.F.);
#6417=ADVANCED_FACE('',(#2038),#6060,.F.);
#6418=ADVANCED_FACE('',(#2039),#6061,.F.);
#6419=ADVANCED_FACE('',(#2040),#6062,.F.);
#6420=ADVANCED_FACE('',(#2041,#1685),#6063,.T.);
#6421=ADVANCED_FACE('',(#2042),#1615,.T.);
#6422=ADVANCED_FACE('',(#2043,#1686),#6064,.F.);
#6423=ADVANCED_FACE('',(#2044),#6065,.T.);
#6424=CLOSED_SHELL('',(#6066,#6067,#6068,#6069,#6070,#6071,#6072,#6073,
#6074,#6075,#6076,#6077,#6078,#6079,#6080,#6081,#6082,#6083,#6084,#6085,
#6086,#6087,#6088,#6089,#6090,#6091,#6092,#6093,#6094,#6095,#6096,#6097));
#6425=CLOSED_SHELL('',(#6098,#6099,#6100,#6101,#6102,#6103,#6104,#6105,
#6106,#6107,#6108,#6109,#6110,#6111,#6112,#6113,#6114,#6115,#6116,#6117,
#6118,#6119,#6120,#6121,#6122,#6123,#6124,#6125,#6126,#6127,#6128,#6129,
#6130,#6131,#6132,#6133,#6134,#6135,#6136,#6137,#6138,#6139,#6140,#6141,
#6142,#6143,#6144,#6145,#6146,#6147,#6148,#6149,#6150,#6151,#6152,#6153,
#6154,#6155,#6156,#6157,#6158,#6159,#6160,#6161,#6162,#6163,#6164,#6165,
#6166,#6167,#6168,#6169,#6170,#6171,#6172,#6173,#6174,#6175,#6176,#6177,
#6178,#6179,#6180,#6181,#6182,#6183,#6184,#6185,#6186,#6187,#6188,#6189,
#6190,#6191,#6192,#6193,#6194,#6195,#6196,#6197,#6198,#6199,#6200,#6201,
#6202,#6203,#6204,#6205,#6206,#6207,#6208));
#6426=CLOSED_SHELL('',(#6209,#6210,#6211,#6212,#6213,#6214,#6215,#6216,
#6217,#6218,#6219,#6220,#6221,#6222,#6223,#6224,#6225,#6226,#6227,#6228,
#6229,#6230,#6231,#6232,#6233,#6234,#6235,#6236,#6237,#6238,#6239,#6240,
#6241,#6242,#6243,#6244,#6245,#6246,#6247,#6248,#6249,#6250,#6251,#6252,
#6253));
#6427=CLOSED_SHELL('',(#6254,#6255,#6256,#6257,#6258,#6259,#6260,#6261,
#6262,#6263,#6264,#6265,#6266,#6267,#6268,#6269,#6270,#6271,#6272,#6273,
#6274,#6275));
#6428=CLOSED_SHELL('',(#6276,#6277,#6278,#6279,#6280,#6281,#6282,#6283,
#6284));
#6429=CLOSED_SHELL('',(#6285,#6286,#6287,#6288,#6289,#6290,#6291,#6292,
#6293));
#6430=CLOSED_SHELL('',(#6294,#6295,#6296,#6297));
#6431=CLOSED_SHELL('',(#6298,#6299,#6300,#6301,#6302,#6303));
#6432=CLOSED_SHELL('',(#6304,#6305,#6306,#6307));
#6433=CLOSED_SHELL('',(#6308,#6309,#6310,#6311));
#6434=CLOSED_SHELL('',(#6312,#6313,#6314,#6315));
#6435=CLOSED_SHELL('',(#6316,#6317,#6318,#6319,#6320,#6321));
#6436=CLOSED_SHELL('',(#6322,#6323,#6324,#6325,#6326,#6327,#6328,#6329,
#6330));
#6437=CLOSED_SHELL('',(#6331,#6332,#6333,#6334));
#6438=CLOSED_SHELL('',(#6335,#6336,#6337,#6338));
#6439=CLOSED_SHELL('',(#6339,#6340,#6341,#6342,#6343,#6344));
#6440=CLOSED_SHELL('',(#6345,#6346,#6347,#6348));
#6441=CLOSED_SHELL('',(#6349,#6350,#6351,#6352,#6353,#6354,#6355,#6356,
#6357,#6358,#6359,#6360,#6361,#6362,#6363,#6364,#6365,#6366,#6367,#6368,
#6369,#6370,#6371,#6372,#6373,#6374,#6375,#6376,#6377,#6378,#6379,#6380,
#6381));
#6442=CLOSED_SHELL('',(#6382,#6383,#6384,#6385,#6386,#6387,#6388,#6389,
#6390,#6391,#6392,#6393,#6394,#6395,#6396,#6397,#6398,#6399,#6400,#6401,
#6402,#6403,#6404,#6405,#6406,#6407,#6408,#6409,#6410,#6411,#6412,#6413,
#6414,#6415,#6416,#6417,#6418,#6419,#6420,#6421,#6422,#6423));
#6443=DERIVED_UNIT_ELEMENT(#6481,1.);
#6444=DERIVED_UNIT_ELEMENT(#19865,-3.);
#6445=DERIVED_UNIT_ELEMENT(#6481,1.);
#6446=DERIVED_UNIT_ELEMENT(#19865,-3.);
#6447=DERIVED_UNIT_ELEMENT(#6481,1.);
#6448=DERIVED_UNIT_ELEMENT(#19865,-3.);
#6449=DERIVED_UNIT_ELEMENT(#6481,1.);
#6450=DERIVED_UNIT_ELEMENT(#19865,-3.);
#6451=DERIVED_UNIT_ELEMENT(#6481,1.);
#6452=DERIVED_UNIT_ELEMENT(#19865,-3.);
#6453=DERIVED_UNIT_ELEMENT(#6481,1.);
#6454=DERIVED_UNIT_ELEMENT(#19865,-3.);
#6455=DERIVED_UNIT_ELEMENT(#6481,1.);
#6456=DERIVED_UNIT_ELEMENT(#19865,-3.);
#6457=DERIVED_UNIT_ELEMENT(#6481,1.);
#6458=DERIVED_UNIT_ELEMENT(#19865,-3.);
#6459=DERIVED_UNIT_ELEMENT(#6481,1.);
#6460=DERIVED_UNIT_ELEMENT(#19865,-3.);
#6461=DERIVED_UNIT_ELEMENT(#6481,1.);
#6462=DERIVED_UNIT_ELEMENT(#19865,-3.);
#6463=DERIVED_UNIT_ELEMENT(#6481,1.);
#6464=DERIVED_UNIT_ELEMENT(#19865,-3.);
#6465=DERIVED_UNIT_ELEMENT(#6481,1.);
#6466=DERIVED_UNIT_ELEMENT(#19865,-3.);
#6467=DERIVED_UNIT_ELEMENT(#6481,1.);
#6468=DERIVED_UNIT_ELEMENT(#19865,-3.);
#6469=DERIVED_UNIT_ELEMENT(#6481,1.);
#6470=DERIVED_UNIT_ELEMENT(#19865,-3.);
#6471=DERIVED_UNIT_ELEMENT(#6481,1.);
#6472=DERIVED_UNIT_ELEMENT(#19865,-3.);
#6473=DERIVED_UNIT_ELEMENT(#6481,1.);
#6474=DERIVED_UNIT_ELEMENT(#19865,-3.);
#6475=DERIVED_UNIT_ELEMENT(#6481,1.);
#6476=DERIVED_UNIT_ELEMENT(#19865,-3.);
#6477=DERIVED_UNIT_ELEMENT(#6481,1.);
#6478=DERIVED_UNIT_ELEMENT(#19865,-3.);
#6479=DERIVED_UNIT_ELEMENT(#6481,1.);
#6480=DERIVED_UNIT_ELEMENT(#19865,-3.);
#6481=(
MASS_UNIT()
NAMED_UNIT(*)
SI_UNIT(.KILO.,.GRAM.)
);
#6482=DERIVED_UNIT((#6443,#6444));
#6483=DERIVED_UNIT((#6445,#6446));
#6484=DERIVED_UNIT((#6447,#6448));
#6485=DERIVED_UNIT((#6449,#6450));
#6486=DERIVED_UNIT((#6451,#6452));
#6487=DERIVED_UNIT((#6453,#6454));
#6488=DERIVED_UNIT((#6455,#6456));
#6489=DERIVED_UNIT((#6457,#6458));
#6490=DERIVED_UNIT((#6459,#6460));
#6491=DERIVED_UNIT((#6461,#6462));
#6492=DERIVED_UNIT((#6463,#6464));
#6493=DERIVED_UNIT((#6465,#6466));
#6494=DERIVED_UNIT((#6467,#6468));
#6495=DERIVED_UNIT((#6469,#6470));
#6496=DERIVED_UNIT((#6471,#6472));
#6497=DERIVED_UNIT((#6473,#6474));
#6498=DERIVED_UNIT((#6475,#6476));
#6499=DERIVED_UNIT((#6477,#6478));
#6500=DERIVED_UNIT((#6479,#6480));
#6501=MEASURE_REPRESENTATION_ITEM('density measure',
POSITIVE_RATIO_MEASURE(7850.),#6482);
#6502=MEASURE_REPRESENTATION_ITEM('density measure',
POSITIVE_RATIO_MEASURE(7850.),#6483);
#6503=MEASURE_REPRESENTATION_ITEM('density measure',
POSITIVE_RATIO_MEASURE(7850.),#6484);
#6504=MEASURE_REPRESENTATION_ITEM('density measure',
POSITIVE_RATIO_MEASURE(7850.),#6485);
#6505=MEASURE_REPRESENTATION_ITEM('density measure',
POSITIVE_RATIO_MEASURE(7850.),#6486);
#6506=MEASURE_REPRESENTATION_ITEM('density measure',
POSITIVE_RATIO_MEASURE(7850.),#6487);
#6507=MEASURE_REPRESENTATION_ITEM('density measure',
POSITIVE_RATIO_MEASURE(7850.),#6488);
#6508=MEASURE_REPRESENTATION_ITEM('density measure',
POSITIVE_RATIO_MEASURE(7850.),#6489);
#6509=MEASURE_REPRESENTATION_ITEM('density measure',
POSITIVE_RATIO_MEASURE(8920.),#6490);
#6510=MEASURE_REPRESENTATION_ITEM('density measure',
POSITIVE_RATIO_MEASURE(7850.),#6491);
#6511=MEASURE_REPRESENTATION_ITEM('density measure',
POSITIVE_RATIO_MEASURE(7850.),#6492);
#6512=MEASURE_REPRESENTATION_ITEM('density measure',
POSITIVE_RATIO_MEASURE(7850.),#6493);
#6513=MEASURE_REPRESENTATION_ITEM('density measure',
POSITIVE_RATIO_MEASURE(7850.),#6494);
#6514=MEASURE_REPRESENTATION_ITEM('density measure',
POSITIVE_RATIO_MEASURE(7850.),#6495);
#6515=MEASURE_REPRESENTATION_ITEM('density measure',
POSITIVE_RATIO_MEASURE(7850.),#6496);
#6516=MEASURE_REPRESENTATION_ITEM('density measure',
POSITIVE_RATIO_MEASURE(7850.),#6497);
#6517=MEASURE_REPRESENTATION_ITEM('density measure',
POSITIVE_RATIO_MEASURE(1425.),#6498);
#6518=MEASURE_REPRESENTATION_ITEM('density measure',
POSITIVE_RATIO_MEASURE(7850.),#6499);
#6519=MEASURE_REPRESENTATION_ITEM('density measure',
POSITIVE_RATIO_MEASURE(7850.),#6500);
#6520=PROPERTY_DEFINITION_REPRESENTATION(#6615,#6558);
#6521=PROPERTY_DEFINITION_REPRESENTATION(#6616,#6559);
#6522=PROPERTY_DEFINITION_REPRESENTATION(#6617,#6560);
#6523=PROPERTY_DEFINITION_REPRESENTATION(#6618,#6561);
#6524=PROPERTY_DEFINITION_REPRESENTATION(#6619,#6562);
#6525=PROPERTY_DEFINITION_REPRESENTATION(#6620,#6563);
#6526=PROPERTY_DEFINITION_REPRESENTATION(#6621,#6564);
#6527=PROPERTY_DEFINITION_REPRESENTATION(#6622,#6565);
#6528=PROPERTY_DEFINITION_REPRESENTATION(#6623,#6566);
#6529=PROPERTY_DEFINITION_REPRESENTATION(#6624,#6567);
#6530=PROPERTY_DEFINITION_REPRESENTATION(#6625,#6568);
#6531=PROPERTY_DEFINITION_REPRESENTATION(#6626,#6569);
#6532=PROPERTY_DEFINITION_REPRESENTATION(#6627,#6570);
#6533=PROPERTY_DEFINITION_REPRESENTATION(#6628,#6571);
#6534=PROPERTY_DEFINITION_REPRESENTATION(#6629,#6572);
#6535=PROPERTY_DEFINITION_REPRESENTATION(#6630,#6573);
#6536=PROPERTY_DEFINITION_REPRESENTATION(#6631,#6574);
#6537=PROPERTY_DEFINITION_REPRESENTATION(#6632,#6575);
#6538=PROPERTY_DEFINITION_REPRESENTATION(#6633,#6576);
#6539=PROPERTY_DEFINITION_REPRESENTATION(#6634,#6577);
#6540=PROPERTY_DEFINITION_REPRESENTATION(#6635,#6578);
#6541=PROPERTY_DEFINITION_REPRESENTATION(#6636,#6579);
#6542=PROPERTY_DEFINITION_REPRESENTATION(#6637,#6580);
#6543=PROPERTY_DEFINITION_REPRESENTATION(#6638,#6581);
#6544=PROPERTY_DEFINITION_REPRESENTATION(#6639,#6582);
#6545=PROPERTY_DEFINITION_REPRESENTATION(#6640,#6583);
#6546=PROPERTY_DEFINITION_REPRESENTATION(#6641,#6584);
#6547=PROPERTY_DEFINITION_REPRESENTATION(#6642,#6585);
#6548=PROPERTY_DEFINITION_REPRESENTATION(#6643,#6586);
#6549=PROPERTY_DEFINITION_REPRESENTATION(#6644,#6587);
#6550=PROPERTY_DEFINITION_REPRESENTATION(#6645,#6588);
#6551=PROPERTY_DEFINITION_REPRESENTATION(#6646,#6589);
#6552=PROPERTY_DEFINITION_REPRESENTATION(#6647,#6590);
#6553=PROPERTY_DEFINITION_REPRESENTATION(#6648,#6591);
#6554=PROPERTY_DEFINITION_REPRESENTATION(#6649,#6592);
#6555=PROPERTY_DEFINITION_REPRESENTATION(#6650,#6593);
#6556=PROPERTY_DEFINITION_REPRESENTATION(#6651,#6594);
#6557=PROPERTY_DEFINITION_REPRESENTATION(#6652,#6595);
#6558=REPRESENTATION('material name',(#6596),#19844);
#6559=REPRESENTATION('density',(#6501),#19844);
#6560=REPRESENTATION('material name',(#6597),#19845);
#6561=REPRESENTATION('density',(#6502),#19845);
#6562=REPRESENTATION('material name',(#6598),#19846);
#6563=REPRESENTATION('density',(#6503),#19846);
#6564=REPRESENTATION('material name',(#6599),#19847);
#6565=REPRESENTATION('density',(#6504),#19847);
#6566=REPRESENTATION('material name',(#6600),#19848);
#6567=REPRESENTATION('density',(#6505),#19848);
#6568=REPRESENTATION('material name',(#6601),#19849);
#6569=REPRESENTATION('density',(#6506),#19849);
#6570=REPRESENTATION('material name',(#6602),#19850);
#6571=REPRESENTATION('density',(#6507),#19850);
#6572=REPRESENTATION('material name',(#6603),#19851);
#6573=REPRESENTATION('density',(#6508),#19851);
#6574=REPRESENTATION('material name',(#6604),#19852);
#6575=REPRESENTATION('density',(#6509),#19852);
#6576=REPRESENTATION('material name',(#6605),#19853);
#6577=REPRESENTATION('density',(#6510),#19853);
#6578=REPRESENTATION('material name',(#6606),#19854);
#6579=REPRESENTATION('density',(#6511),#19854);
#6580=REPRESENTATION('material name',(#6607),#19855);
#6581=REPRESENTATION('density',(#6512),#19855);
#6582=REPRESENTATION('material name',(#6608),#19856);
#6583=REPRESENTATION('density',(#6513),#19856);
#6584=REPRESENTATION('material name',(#6609),#19857);
#6585=REPRESENTATION('density',(#6514),#19857);
#6586=REPRESENTATION('material name',(#6610),#19858);
#6587=REPRESENTATION('density',(#6515),#19858);
#6588=REPRESENTATION('material name',(#6611),#19859);
#6589=REPRESENTATION('density',(#6516),#19859);
#6590=REPRESENTATION('material name',(#6612),#19860);
#6591=REPRESENTATION('density',(#6517),#19860);
#6592=REPRESENTATION('material name',(#6613),#19861);
#6593=REPRESENTATION('density',(#6518),#19861);
#6594=REPRESENTATION('material name',(#6614),#19862);
#6595=REPRESENTATION('density',(#6519),#19862);
#6596=DESCRIPTIVE_REPRESENTATION_ITEM('Steel','Steel');
#6597=DESCRIPTIVE_REPRESENTATION_ITEM('Steel','Steel');
#6598=DESCRIPTIVE_REPRESENTATION_ITEM('Steel','Steel');
#6599=DESCRIPTIVE_REPRESENTATION_ITEM('Steel','Steel');
#6600=DESCRIPTIVE_REPRESENTATION_ITEM('Steel','Steel');
#6601=DESCRIPTIVE_REPRESENTATION_ITEM('Steel','Steel');
#6602=DESCRIPTIVE_REPRESENTATION_ITEM('Steel','Steel');
#6603=DESCRIPTIVE_REPRESENTATION_ITEM('Steel','Steel');
#6604=DESCRIPTIVE_REPRESENTATION_ITEM('Copper, Alloy','Copper, Alloy');
#6605=DESCRIPTIVE_REPRESENTATION_ITEM('Steel','Steel');
#6606=DESCRIPTIVE_REPRESENTATION_ITEM('Steel','Steel');
#6607=DESCRIPTIVE_REPRESENTATION_ITEM('Steel','Steel');
#6608=DESCRIPTIVE_REPRESENTATION_ITEM('Steel','Steel');
#6609=DESCRIPTIVE_REPRESENTATION_ITEM('Steel','Steel');
#6610=DESCRIPTIVE_REPRESENTATION_ITEM('Steel','Steel');
#6611=DESCRIPTIVE_REPRESENTATION_ITEM('Steel','Steel');
#6612=DESCRIPTIVE_REPRESENTATION_ITEM('Acetal Resin, White',
'Acetal Resin, White');
#6613=DESCRIPTIVE_REPRESENTATION_ITEM('Steel','Steel');
#6614=DESCRIPTIVE_REPRESENTATION_ITEM('Steel','Steel');
#6615=PROPERTY_DEFINITION('material property','material name',#19956);
#6616=PROPERTY_DEFINITION('material property','density of part',#19956);
#6617=PROPERTY_DEFINITION('material property','material name',#19957);
#6618=PROPERTY_DEFINITION('material property','density of part',#19957);
#6619=PROPERTY_DEFINITION('material property','material name',#19958);
#6620=PROPERTY_DEFINITION('material property','density of part',#19958);
#6621=PROPERTY_DEFINITION('material property','material name',#19959);
#6622=PROPERTY_DEFINITION('material property','density of part',#19959);
#6623=PROPERTY_DEFINITION('material property','material name',#19960);
#6624=PROPERTY_DEFINITION('material property','density of part',#19960);
#6625=PROPERTY_DEFINITION('material property','material name',#19961);
#6626=PROPERTY_DEFINITION('material property','density of part',#19961);
#6627=PROPERTY_DEFINITION('material property','material name',#19962);
#6628=PROPERTY_DEFINITION('material property','density of part',#19962);
#6629=PROPERTY_DEFINITION('material property','material name',#19963);
#6630=PROPERTY_DEFINITION('material property','density of part',#19963);
#6631=PROPERTY_DEFINITION('material property','material name',#19964);
#6632=PROPERTY_DEFINITION('material property','density of part',#19964);
#6633=PROPERTY_DEFINITION('material property','material name',#19965);
#6634=PROPERTY_DEFINITION('material property','density of part',#19965);
#6635=PROPERTY_DEFINITION('material property','material name',#19966);
#6636=PROPERTY_DEFINITION('material property','density of part',#19966);
#6637=PROPERTY_DEFINITION('material property','material name',#19967);
#6638=PROPERTY_DEFINITION('material property','density of part',#19967);
#6639=PROPERTY_DEFINITION('material property','material name',#19968);
#6640=PROPERTY_DEFINITION('material property','density of part',#19968);
#6641=PROPERTY_DEFINITION('material property','material name',#19969);
#6642=PROPERTY_DEFINITION('material property','density of part',#19969);
#6643=PROPERTY_DEFINITION('material property','material name',#19970);
#6644=PROPERTY_DEFINITION('material property','density of part',#19970);
#6645=PROPERTY_DEFINITION('material property','material name',#19971);
#6646=PROPERTY_DEFINITION('material property','density of part',#19971);
#6647=PROPERTY_DEFINITION('material property','material name',#19972);
#6648=PROPERTY_DEFINITION('material property','density of part',#19972);
#6649=PROPERTY_DEFINITION('material property','material name',#19973);
#6650=PROPERTY_DEFINITION('material property','density of part',#19973);
#6651=PROPERTY_DEFINITION('material property','material name',#19974);
#6652=PROPERTY_DEFINITION('material property','density of part',#19974);
#6653=AXIS2_PLACEMENT_3D('',#8732,#7191,#7192);
#6654=AXIS2_PLACEMENT_3D('',#8733,#7193,#7194);
#6655=AXIS2_PLACEMENT_3D('',#8734,#7195,#7196);
#6656=AXIS2_PLACEMENT_3D('',#8736,#7197,#7198);
#6657=AXIS2_PLACEMENT_3D('',#8738,#7199,#7200);
#6658=AXIS2_PLACEMENT_3D('',#8739,#7201,#7202);
#6659=AXIS2_PLACEMENT_3D('',#8741,#7203,#7204);
#6660=AXIS2_PLACEMENT_3D('',#8743,#7206,#7207);
#6661=AXIS2_PLACEMENT_3D('',#8746,#7209,#7210);
#6662=AXIS2_PLACEMENT_3D('',#8747,#7211,#7212);
#6663=AXIS2_PLACEMENT_3D('',#8749,#7213,#7214);
#6664=AXIS2_PLACEMENT_3D('',#8751,#7215,#7216);
#6665=AXIS2_PLACEMENT_3D('',#8752,#7217,#7218);
#6666=AXIS2_PLACEMENT_3D('',#8754,#7219,#7220);
#6667=AXIS2_PLACEMENT_3D('',#8756,#7222,#7223);
#6668=AXIS2_PLACEMENT_3D('',#8759,#7225,#7226);
#6669=AXIS2_PLACEMENT_3D('',#8760,#7227,#7228);
#6670=AXIS2_PLACEMENT_3D('',#8762,#7229,#7230);
#6671=AXIS2_PLACEMENT_3D('',#8765,#7232,#7233);
#6672=AXIS2_PLACEMENT_3D('',#8766,#7234,#7235);
#6673=AXIS2_PLACEMENT_3D('',#8768,#7236,#7237);
#6674=AXIS2_PLACEMENT_3D('',#8771,#7239,#7240);
#6675=AXIS2_PLACEMENT_3D('',#8772,#7241,#7242);
#6676=AXIS2_PLACEMENT_3D('',#8774,#7243,#7244);
#6677=AXIS2_PLACEMENT_3D('',#8777,#7246,#7247);
#6678=AXIS2_PLACEMENT_3D('',#8778,#7248,#7249);
#6679=AXIS2_PLACEMENT_3D('',#8780,#7250,#7251);
#6680=AXIS2_PLACEMENT_3D('',#8783,#7253,#7254);
#6681=AXIS2_PLACEMENT_3D('',#8784,#7255,#7256);
#6682=AXIS2_PLACEMENT_3D('',#8793,#7261,#7262);
#6683=AXIS2_PLACEMENT_3D('',#8799,#7266,#7267);
#6684=AXIS2_PLACEMENT_3D('',#8805,#7271,#7272);
#6685=AXIS2_PLACEMENT_3D('',#8808,#7275,#7276);
#6686=AXIS2_PLACEMENT_3D('',#8817,#7281,#7282);
#6687=AXIS2_PLACEMENT_3D('',#8823,#7286,#7287);
#6688=AXIS2_PLACEMENT_3D('',#8829,#7291,#7292);
#6689=AXIS2_PLACEMENT_3D('',#8832,#7295,#7296);
#6690=AXIS2_PLACEMENT_3D('',#8841,#7301,#7302);
#6691=AXIS2_PLACEMENT_3D('',#8850,#7307,#7308);
#6692=AXIS2_PLACEMENT_3D('',#8853,#7311,#7312);
#6693=AXIS2_PLACEMENT_3D('',#8859,#7316,#7317);
#6694=AXIS2_PLACEMENT_3D('',#8865,#7321,#7322);
#6695=AXIS2_PLACEMENT_3D('',#8871,#7326,#7327);
#6696=AXIS2_PLACEMENT_3D('',#8880,#7332,#7333);
#6697=AXIS2_PLACEMENT_3D('',#8883,#7336,#7337);
#6698=AXIS2_PLACEMENT_3D('',#8889,#7341,#7342);
#6699=AXIS2_PLACEMENT_3D('',#8895,#7346,#7347);
#6700=AXIS2_PLACEMENT_3D('',#8899,#7350,#7351);
#6701=AXIS2_PLACEMENT_3D('',#8903,#7354,#7355);
#6702=AXIS2_PLACEMENT_3D('',#8905,#7357,#7358);
#6703=AXIS2_PLACEMENT_3D('',#8906,#7359,#7360);
#6704=AXIS2_PLACEMENT_3D('',#8907,#7361,#7362);
#6705=AXIS2_PLACEMENT_3D('',#8932,#7364,#7365);
#6706=AXIS2_PLACEMENT_3D('',#8940,#7367,#7368);
#6707=AXIS2_PLACEMENT_3D('',#8963,#7369,#7370);
#6708=AXIS2_PLACEMENT_3D('',#9014,#7372,#7373);
#6709=AXIS2_PLACEMENT_3D('',#9062,#7375,#7376);
#6710=AXIS2_PLACEMENT_3D('',#9113,#7378,#7379);
#6711=AXIS2_PLACEMENT_3D('',#9164,#7381,#7382);
#6712=AXIS2_PLACEMENT_3D('',#9212,#7384,#7385);
#6713=AXIS2_PLACEMENT_3D('',#9260,#7387,#7388);
#6714=AXIS2_PLACEMENT_3D('',#9311,#7390,#7391);
#6715=AXIS2_PLACEMENT_3D('',#9359,#7393,#7394);
#6716=AXIS2_PLACEMENT_3D('',#9407,#7396,#7397);
#6717=AXIS2_PLACEMENT_3D('',#9458,#7399,#7400);
#6718=AXIS2_PLACEMENT_3D('',#9509,#7402,#7403);
#6719=AXIS2_PLACEMENT_3D('',#9557,#7405,#7406);
#6720=AXIS2_PLACEMENT_3D('',#9608,#7408,#7409);
#6721=AXIS2_PLACEMENT_3D('',#9627,#7411,#7412);
#6722=AXIS2_PLACEMENT_3D('',#9647,#7413,#7414);
#6723=AXIS2_PLACEMENT_3D('',#9659,#7416,#7417);
#6724=AXIS2_PLACEMENT_3D('',#9667,#7418,#7419);
#6725=AXIS2_PLACEMENT_3D('',#9691,#7421,#7422);
#6726=AXIS2_PLACEMENT_3D('',#9716,#7424,#7425);
#6727=AXIS2_PLACEMENT_3D('',#9741,#7427,#7428);
#6728=AXIS2_PLACEMENT_3D('',#9765,#7430,#7431);
#6729=AXIS2_PLACEMENT_3D('',#9790,#7433,#7434);
#6730=AXIS2_PLACEMENT_3D('',#9814,#7436,#7437);
#6731=AXIS2_PLACEMENT_3D('',#9839,#7439,#7440);
#6732=AXIS2_PLACEMENT_3D('',#9864,#7442,#7443);
#6733=AXIS2_PLACEMENT_3D('',#9888,#7445,#7446);
#6734=AXIS2_PLACEMENT_3D('',#9913,#7448,#7449);
#6735=AXIS2_PLACEMENT_3D('',#9937,#7451,#7452);
#6736=AXIS2_PLACEMENT_3D('',#9962,#7454,#7455);
#6737=AXIS2_PLACEMENT_3D('',#9987,#7457,#7458);
#6738=AXIS2_PLACEMENT_3D('',#10011,#7460,#7461);
#6739=AXIS2_PLACEMENT_3D('',#10022,#7463,#7464);
#6740=AXIS2_PLACEMENT_3D('',#10028,#7465,#7466);
#6741=AXIS2_PLACEMENT_3D('',#10053,#7468,#7469);
#6742=AXIS2_PLACEMENT_3D('',#10061,#7471,#7472);
#6743=AXIS2_PLACEMENT_3D('',#10084,#7473,#7474);
#6744=AXIS2_PLACEMENT_3D('',#10135,#7476,#7477);
#6745=AXIS2_PLACEMENT_3D('',#10183,#7479,#7480);
#6746=AXIS2_PLACEMENT_3D('',#10234,#7482,#7483);
#6747=AXIS2_PLACEMENT_3D('',#10285,#7485,#7486);
#6748=AXIS2_PLACEMENT_3D('',#10333,#7488,#7489);
#6749=AXIS2_PLACEMENT_3D('',#10381,#7491,#7492);
#6750=AXIS2_PLACEMENT_3D('',#10432,#7494,#7495);
#6751=AXIS2_PLACEMENT_3D('',#10480,#7497,#7498);
#6752=AXIS2_PLACEMENT_3D('',#10528,#7500,#7501);
#6753=AXIS2_PLACEMENT_3D('',#10579,#7503,#7504);
#6754=AXIS2_PLACEMENT_3D('',#10630,#7506,#7507);
#6755=AXIS2_PLACEMENT_3D('',#10678,#7509,#7510);
#6756=AXIS2_PLACEMENT_3D('',#10729,#7512,#7513);
#6757=AXIS2_PLACEMENT_3D('',#10748,#7515,#7516);
#6758=AXIS2_PLACEMENT_3D('',#10768,#7517,#7518);
#6759=AXIS2_PLACEMENT_3D('',#10780,#7520,#7521);
#6760=AXIS2_PLACEMENT_3D('',#10788,#7522,#7523);
#6761=AXIS2_PLACEMENT_3D('',#10812,#7525,#7526);
#6762=AXIS2_PLACEMENT_3D('',#10837,#7528,#7529);
#6763=AXIS2_PLACEMENT_3D('',#10862,#7531,#7532);
#6764=AXIS2_PLACEMENT_3D('',#10886,#7534,#7535);
#6765=AXIS2_PLACEMENT_3D('',#10911,#7537,#7538);
#6766=AXIS2_PLACEMENT_3D('',#10935,#7540,#7541);
#6767=AXIS2_PLACEMENT_3D('',#10960,#7543,#7544);
#6768=AXIS2_PLACEMENT_3D('',#10985,#7546,#7547);
#6769=AXIS2_PLACEMENT_3D('',#11009,#7549,#7550);
#6770=AXIS2_PLACEMENT_3D('',#11034,#7552,#7553);
#6771=AXIS2_PLACEMENT_3D('',#11058,#7555,#7556);
#6772=AXIS2_PLACEMENT_3D('',#11083,#7558,#7559);
#6773=AXIS2_PLACEMENT_3D('',#11108,#7561,#7562);
#6774=AXIS2_PLACEMENT_3D('',#11132,#7564,#7565);
#6775=AXIS2_PLACEMENT_3D('',#11143,#7567,#7568);
#6776=AXIS2_PLACEMENT_3D('',#11149,#7569,#7570);
#6777=AXIS2_PLACEMENT_3D('',#11323,#7571,#7572);
#6778=AXIS2_PLACEMENT_3D('',#12391,#7573,#7574);
#6779=AXIS2_PLACEMENT_3D('',#12392,#7575,#7576);
#6780=AXIS2_PLACEMENT_3D('',#12566,#7577,#7578);
#6781=AXIS2_PLACEMENT_3D('',#13634,#7579,#7580);
#6782=AXIS2_PLACEMENT_3D('',#13635,#7581,#7582);
#6783=AXIS2_PLACEMENT_3D('',#13636,#7583,#7584);
#6784=AXIS2_PLACEMENT_3D('',#13637,#7585,#7586);
#6785=AXIS2_PLACEMENT_3D('',#13639,#7587,#7588);
#6786=AXIS2_PLACEMENT_3D('',#13642,#7590,#7591);
#6787=AXIS2_PLACEMENT_3D('',#13643,#7592,#7593);
#6788=AXIS2_PLACEMENT_3D('',#13645,#7594,#7595);
#6789=AXIS2_PLACEMENT_3D('',#13648,#7597,#7598);
#6790=AXIS2_PLACEMENT_3D('',#13649,#7599,#7600);
#6791=AXIS2_PLACEMENT_3D('',#13651,#7601,#7602);
#6792=AXIS2_PLACEMENT_3D('',#13654,#7604,#7605);
#6793=AXIS2_PLACEMENT_3D('',#13655,#7606,#7607);
#6794=AXIS2_PLACEMENT_3D('',#13664,#7612,#7613);
#6795=AXIS2_PLACEMENT_3D('',#13673,#7618,#7619);
#6796=AXIS2_PLACEMENT_3D('',#13676,#7622,#7623);
#6797=AXIS2_PLACEMENT_3D('',#13682,#7627,#7628);
#6798=AXIS2_PLACEMENT_3D('',#13688,#7632,#7633);
#6799=AXIS2_PLACEMENT_3D('',#13697,#7638,#7639);
#6800=AXIS2_PLACEMENT_3D('',#13703,#7643,#7644);
#6801=AXIS2_PLACEMENT_3D('',#13709,#7648,#7649);
#6802=AXIS2_PLACEMENT_3D('',#13711,#7651,#7652);
#6803=AXIS2_PLACEMENT_3D('',#13745,#7670,#7671);
#6804=AXIS2_PLACEMENT_3D('',#13748,#7674,#7675);
#6805=AXIS2_PLACEMENT_3D('',#13750,#7677,#7678);
#6806=AXIS2_PLACEMENT_3D('',#13752,#7680,#7681);
#6807=AXIS2_PLACEMENT_3D('',#13766,#7689,#7690);
#6808=AXIS2_PLACEMENT_3D('',#13772,#7694,#7695);
#6809=AXIS2_PLACEMENT_3D('',#13776,#7698,#7699);
#6810=AXIS2_PLACEMENT_3D('',#13780,#7702,#7703);
#6811=AXIS2_PLACEMENT_3D('',#13782,#7705,#7706);
#6812=AXIS2_PLACEMENT_3D('',#13788,#7710,#7711);
#6813=AXIS2_PLACEMENT_3D('',#13792,#7714,#7715);
#6814=AXIS2_PLACEMENT_3D('',#13796,#7718,#7719);
#6815=AXIS2_PLACEMENT_3D('',#13798,#7721,#7722);
#6816=AXIS2_PLACEMENT_3D('',#13812,#7730,#7731);
#6817=AXIS2_PLACEMENT_3D('',#13816,#7734,#7735);
#6818=AXIS2_PLACEMENT_3D('',#13822,#7739,#7740);
#6819=AXIS2_PLACEMENT_3D('',#13826,#7743,#7744);
#6820=AXIS2_PLACEMENT_3D('',#13833,#7749,#7750);
#6821=AXIS2_PLACEMENT_3D('',#13835,#7752,#7753);
#6822=AXIS2_PLACEMENT_3D('',#13836,#7754,#7755);
#6823=AXIS2_PLACEMENT_3D('',#13840,#7758,#7759);
#6824=AXIS2_PLACEMENT_3D('',#13844,#7762,#7763);
#6825=AXIS2_PLACEMENT_3D('',#13847,#7766,#7767);
#6826=AXIS2_PLACEMENT_3D('',#13848,#7768,#7769);
#6827=AXIS2_PLACEMENT_3D('',#13849,#7770,#7771);
#6828=AXIS2_PLACEMENT_3D('',#13850,#7772,#7773);
#6829=AXIS2_PLACEMENT_3D('',#13860,#7775,#7776);
#6830=AXIS2_PLACEMENT_3D('',#13871,#7777,#7778);
#6831=AXIS2_PLACEMENT_3D('',#13922,#7780,#7781);
#6832=AXIS2_PLACEMENT_3D('',#13973,#7783,#7784);
#6833=AXIS2_PLACEMENT_3D('',#14021,#7786,#7787);
#6834=AXIS2_PLACEMENT_3D('',#14069,#7789,#7790);
#6835=AXIS2_PLACEMENT_3D('',#14120,#7792,#7793);
#6836=AXIS2_PLACEMENT_3D('',#14171,#7795,#7796);
#6837=AXIS2_PLACEMENT_3D('',#14219,#7798,#7799);
#6838=AXIS2_PLACEMENT_3D('',#14270,#7801,#7802);
#6839=AXIS2_PLACEMENT_3D('',#14289,#7804,#7805);
#6840=AXIS2_PLACEMENT_3D('',#14309,#7806,#7807);
#6841=AXIS2_PLACEMENT_3D('',#14323,#7809,#7810);
#6842=AXIS2_PLACEMENT_3D('',#14333,#7811,#7812);
#6843=AXIS2_PLACEMENT_3D('',#14357,#7814,#7815);
#6844=AXIS2_PLACEMENT_3D('',#14382,#7817,#7818);
#6845=AXIS2_PLACEMENT_3D('',#14406,#7820,#7821);
#6846=AXIS2_PLACEMENT_3D('',#14431,#7823,#7824);
#6847=AXIS2_PLACEMENT_3D('',#14455,#7826,#7827);
#6848=AXIS2_PLACEMENT_3D('',#14480,#7829,#7830);
#6849=AXIS2_PLACEMENT_3D('',#14505,#7832,#7833);
#6850=AXIS2_PLACEMENT_3D('',#14529,#7835,#7836);
#6851=AXIS2_PLACEMENT_3D('',#14540,#7838,#7839);
#6852=AXIS2_PLACEMENT_3D('',#14546,#7840,#7841);
#6853=AXIS2_PLACEMENT_3D('',#14549,#7842,#7843);
#6854=AXIS2_PLACEMENT_3D('',#14553,#7845,#7846);
#6855=AXIS2_PLACEMENT_3D('',#14555,#7848,#7849);
#6856=AXIS2_PLACEMENT_3D('',#14557,#7850,#7851);
#6857=AXIS2_PLACEMENT_3D('',#14560,#7853,#7854);
#6858=AXIS2_PLACEMENT_3D('',#14561,#7855,#7856);
#6859=AXIS2_PLACEMENT_3D('',#14563,#7857,#7858);
#6860=AXIS2_PLACEMENT_3D('',#14566,#7860,#7861);
#6861=AXIS2_PLACEMENT_3D('',#14567,#7862,#7863);
#6862=AXIS2_PLACEMENT_3D('',#14568,#7864,#7865);
#6863=AXIS2_PLACEMENT_3D('',#14569,#7866,#7867);
#6864=AXIS2_PLACEMENT_3D('',#14570,#7868,#7869);
#6865=AXIS2_PLACEMENT_3D('',#15565,#7870,#7871);
#6866=AXIS2_PLACEMENT_3D('',#15567,#7872,#7873);
#6867=AXIS2_PLACEMENT_3D('',#15568,#7874,#7875);
#6868=AXIS2_PLACEMENT_3D('',#15569,#7876,#7877);
#6869=AXIS2_PLACEMENT_3D('',#15571,#7878,#7879);
#6870=AXIS2_PLACEMENT_3D('',#15574,#7881,#7882);
#6871=AXIS2_PLACEMENT_3D('',#15575,#7883,#7884);
#6872=AXIS2_PLACEMENT_3D('',#15577,#7885,#7886);
#6873=AXIS2_PLACEMENT_3D('',#15580,#7888,#7889);
#6874=AXIS2_PLACEMENT_3D('',#15581,#7890,#7891);
#6875=AXIS2_PLACEMENT_3D('',#15583,#7892,#7893);
#6876=AXIS2_PLACEMENT_3D('',#15586,#7895,#7896);
#6877=AXIS2_PLACEMENT_3D('',#15587,#7897,#7898);
#6878=AXIS2_PLACEMENT_3D('',#15590,#7900,#7901);
#6879=AXIS2_PLACEMENT_3D('',#15591,#7902,#7903);
#6880=AXIS2_PLACEMENT_3D('',#15596,#7905,#7906);
#6881=AXIS2_PLACEMENT_3D('',#15599,#7908,#7909);
#6882=AXIS2_PLACEMENT_3D('',#15600,#7910,#7911);
#6883=AXIS2_PLACEMENT_3D('',#15606,#7914,#7915);
#6884=AXIS2_PLACEMENT_3D('',#15610,#7917,#7918);
#6885=AXIS2_PLACEMENT_3D('',#15614,#7920,#7921);
#6886=AXIS2_PLACEMENT_3D('',#15618,#7924,#7925);
#6887=AXIS2_PLACEMENT_3D('',#15622,#7928,#7929);
#6888=AXIS2_PLACEMENT_3D('',#15626,#7932,#7933);
#6889=AXIS2_PLACEMENT_3D('',#15630,#7936,#7937);
#6890=AXIS2_PLACEMENT_3D('',#15634,#7939,#7940);
#6891=AXIS2_PLACEMENT_3D('',#15638,#7942,#7943);
#6892=AXIS2_PLACEMENT_3D('',#15641,#7945,#7946);
#6893=AXIS2_PLACEMENT_3D('',#15642,#7947,#7948);
#6894=AXIS2_PLACEMENT_3D('',#15645,#7951,#7952);
#6895=AXIS2_PLACEMENT_3D('',#15647,#7954,#7955);
#6896=AXIS2_PLACEMENT_3D('',#15649,#7957,#7958);
#6897=AXIS2_PLACEMENT_3D('',#15651,#7960,#7961);
#6898=AXIS2_PLACEMENT_3D('',#15652,#7962,#7963);
#6899=AXIS2_PLACEMENT_3D('',#15653,#7964,#7965);
#6900=AXIS2_PLACEMENT_3D('',#15654,#7966,#7967);
#6901=AXIS2_PLACEMENT_3D('',#15663,#7972,#7973);
#6902=AXIS2_PLACEMENT_3D('',#15665,#7974,#7975);
#6903=AXIS2_PLACEMENT_3D('',#15668,#7977,#7978);
#6904=AXIS2_PLACEMENT_3D('',#15669,#7979,#7980);
#6905=AXIS2_PLACEMENT_3D('',#15675,#7984,#7985);
#6906=AXIS2_PLACEMENT_3D('',#15676,#7986,#7987);
#6907=AXIS2_PLACEMENT_3D('',#15677,#7988,#7989);
#6908=AXIS2_PLACEMENT_3D('',#15678,#7990,#7991);
#6909=AXIS2_PLACEMENT_3D('',#15687,#7996,#7997);
#6910=AXIS2_PLACEMENT_3D('',#15696,#8002,#8003);
#6911=AXIS2_PLACEMENT_3D('',#15702,#8007,#8008);
#6912=AXIS2_PLACEMENT_3D('',#15707,#8012,#8013);
#6913=AXIS2_PLACEMENT_3D('',#15711,#8016,#8017);
#6914=AXIS2_PLACEMENT_3D('',#15714,#8020,#8021);
#6915=AXIS2_PLACEMENT_3D('',#15715,#8022,#8023);
#6916=AXIS2_PLACEMENT_3D('',#15721,#8027,#8028);
#6917=AXIS2_PLACEMENT_3D('',#15727,#8032,#8033);
#6918=AXIS2_PLACEMENT_3D('',#15733,#8037,#8038);
#6919=AXIS2_PLACEMENT_3D('',#15739,#8042,#8043);
#6920=AXIS2_PLACEMENT_3D('',#15745,#8047,#8048);
#6921=AXIS2_PLACEMENT_3D('',#15753,#8053,#8054);
#6922=AXIS2_PLACEMENT_3D('',#15759,#8058,#8059);
#6923=AXIS2_PLACEMENT_3D('',#15764,#8063,#8064);
#6924=AXIS2_PLACEMENT_3D('',#15766,#8066,#8067);
#6925=AXIS2_PLACEMENT_3D('',#15767,#8068,#8069);
#6926=AXIS2_PLACEMENT_3D('',#15768,#8070,#8071);
#6927=AXIS2_PLACEMENT_3D('',#15769,#8072,#8073);
#6928=AXIS2_PLACEMENT_3D('',#15771,#8074,#8075);
#6929=AXIS2_PLACEMENT_3D('',#15774,#8077,#8078);
#6930=AXIS2_PLACEMENT_3D('',#15775,#8079,#8080);
#6931=AXIS2_PLACEMENT_3D('',#15777,#8081,#8082);
#6932=AXIS2_PLACEMENT_3D('',#15778,#8083,#8084);
#6933=AXIS2_PLACEMENT_3D('',#15780,#8085,#8086);
#6934=AXIS2_PLACEMENT_3D('',#15781,#8087,#8088);
#6935=AXIS2_PLACEMENT_3D('',#15783,#8089,#8090);
#6936=AXIS2_PLACEMENT_3D('',#15785,#8092,#8093);
#6937=AXIS2_PLACEMENT_3D('',#15787,#8094,#8095);
#6938=AXIS2_PLACEMENT_3D('',#15789,#8096,#8097);
#6939=AXIS2_PLACEMENT_3D('',#15790,#8098,#8099);
#6940=AXIS2_PLACEMENT_3D('',#15793,#8101,#8102);
#6941=AXIS2_PLACEMENT_3D('',#15794,#8103,#8104);
#6942=AXIS2_PLACEMENT_3D('',#15795,#8105,#8106);
#6943=AXIS2_PLACEMENT_3D('',#15797,#8108,#8109);
#6944=AXIS2_PLACEMENT_3D('',#15798,#8110,#8111);
#6945=AXIS2_PLACEMENT_3D('',#15799,#8112,#8113);
#6946=AXIS2_PLACEMENT_3D('',#15801,#8114,#8115);
#6947=AXIS2_PLACEMENT_3D('',#15804,#8117,#8118);
#6948=AXIS2_PLACEMENT_3D('',#15805,#8119,#8120);
#6949=AXIS2_PLACEMENT_3D('',#15807,#8121,#8122);
#6950=AXIS2_PLACEMENT_3D('',#15808,#8123,#8124);
#6951=AXIS2_PLACEMENT_3D('',#15810,#8125,#8126);
#6952=AXIS2_PLACEMENT_3D('',#15811,#8127,#8128);
#6953=AXIS2_PLACEMENT_3D('',#15813,#8129,#8130);
#6954=AXIS2_PLACEMENT_3D('',#15815,#8132,#8133);
#6955=AXIS2_PLACEMENT_3D('',#15817,#8134,#8135);
#6956=AXIS2_PLACEMENT_3D('',#15819,#8136,#8137);
#6957=AXIS2_PLACEMENT_3D('',#15820,#8138,#8139);
#6958=AXIS2_PLACEMENT_3D('',#15823,#8141,#8142);
#6959=AXIS2_PLACEMENT_3D('',#15824,#8143,#8144);
#6960=AXIS2_PLACEMENT_3D('',#15825,#8145,#8146);
#6961=AXIS2_PLACEMENT_3D('',#15827,#8148,#8149);
#6962=AXIS2_PLACEMENT_3D('',#15828,#8150,#8151);
#6963=AXIS2_PLACEMENT_3D('',#15829,#8152,#8153);
#6964=AXIS2_PLACEMENT_3D('',#15831,#8154,#8155);
#6965=AXIS2_PLACEMENT_3D('',#15834,#8157,#8158);
#6966=AXIS2_PLACEMENT_3D('',#15835,#8159,#8160);
#6967=AXIS2_PLACEMENT_3D('',#15837,#8161,#8162);
#6968=AXIS2_PLACEMENT_3D('',#15840,#8164,#8165);
#6969=AXIS2_PLACEMENT_3D('',#15841,#8166,#8167);
#6970=AXIS2_PLACEMENT_3D('',#15842,#8168,#8169);
#6971=AXIS2_PLACEMENT_3D('',#15843,#8170,#8171);
#6972=AXIS2_PLACEMENT_3D('',#15844,#8172,#8173);
#6973=AXIS2_PLACEMENT_3D('',#15853,#8178,#8179);
#6974=AXIS2_PLACEMENT_3D('',#15862,#8184,#8185);
#6975=AXIS2_PLACEMENT_3D('',#15863,#8186,#8187);
#6976=AXIS2_PLACEMENT_3D('',#15864,#8188,#8189);
#6977=AXIS2_PLACEMENT_3D('',#15865,#8190,#8191);
#6978=AXIS2_PLACEMENT_3D('',#15866,#8192,#8193);
#6979=AXIS2_PLACEMENT_3D('',#15867,#8194,#8195);
#6980=AXIS2_PLACEMENT_3D('',#15868,#8196,#8197);
#6981=AXIS2_PLACEMENT_3D('',#15869,#8198,#8199);
#6982=AXIS2_PLACEMENT_3D('',#15870,#8200,#8201);
#6983=AXIS2_PLACEMENT_3D('',#15871,#8202,#8203);
#6984=AXIS2_PLACEMENT_3D('',#15873,#8204,#8205);
#6985=AXIS2_PLACEMENT_3D('',#15876,#8207,#8208);
#6986=AXIS2_PLACEMENT_3D('',#15877,#8209,#8210);
#6987=AXIS2_PLACEMENT_3D('',#15879,#8211,#8212);
#6988=AXIS2_PLACEMENT_3D('',#15882,#8214,#8215);
#6989=AXIS2_PLACEMENT_3D('',#15883,#8216,#8217);
#6990=AXIS2_PLACEMENT_3D('',#15884,#8218,#8219);
#6991=AXIS2_PLACEMENT_3D('',#15885,#8220,#8221);
#6992=AXIS2_PLACEMENT_3D('',#15886,#8222,#8223);
#6993=AXIS2_PLACEMENT_3D('',#15888,#8224,#8225);
#6994=AXIS2_PLACEMENT_3D('',#15891,#8227,#8228);
#6995=AXIS2_PLACEMENT_3D('',#15892,#8229,#8230);
#6996=AXIS2_PLACEMENT_3D('',#15894,#8231,#8232);
#6997=AXIS2_PLACEMENT_3D('',#15897,#8234,#8235);
#6998=AXIS2_PLACEMENT_3D('',#15898,#8236,#8237);
#6999=AXIS2_PLACEMENT_3D('',#15899,#8238,#8239);
#7000=AXIS2_PLACEMENT_3D('',#15900,#8240,#8241);
#7001=AXIS2_PLACEMENT_3D('',#15901,#8242,#8243);
#7002=AXIS2_PLACEMENT_3D('',#15903,#8244,#8245);
#7003=AXIS2_PLACEMENT_3D('',#15906,#8247,#8248);
#7004=AXIS2_PLACEMENT_3D('',#15907,#8249,#8250);
#7005=AXIS2_PLACEMENT_3D('',#15909,#8251,#8252);
#7006=AXIS2_PLACEMENT_3D('',#15912,#8254,#8255);
#7007=AXIS2_PLACEMENT_3D('',#15913,#8256,#8257);
#7008=AXIS2_PLACEMENT_3D('',#15914,#8258,#8259);
#7009=AXIS2_PLACEMENT_3D('',#15915,#8260,#8261);
#7010=AXIS2_PLACEMENT_3D('',#15916,#8262,#8263);
#7011=AXIS2_PLACEMENT_3D('',#15925,#8268,#8269);
#7012=AXIS2_PLACEMENT_3D('',#15934,#8274,#8275);
#7013=AXIS2_PLACEMENT_3D('',#15935,#8276,#8277);
#7014=AXIS2_PLACEMENT_3D('',#15936,#8278,#8279);
#7015=AXIS2_PLACEMENT_3D('',#15937,#8280,#8281);
#7016=AXIS2_PLACEMENT_3D('',#15938,#8282,#8283);
#7017=AXIS2_PLACEMENT_3D('',#15939,#8284,#8285);
#7018=AXIS2_PLACEMENT_3D('',#15940,#8286,#8287);
#7019=AXIS2_PLACEMENT_3D('',#15941,#8288,#8289);
#7020=AXIS2_PLACEMENT_3D('',#15942,#8290,#8291);
#7021=AXIS2_PLACEMENT_3D('',#15943,#8292,#8293);
#7022=AXIS2_PLACEMENT_3D('',#15945,#8294,#8295);
#7023=AXIS2_PLACEMENT_3D('',#15948,#8297,#8298);
#7024=AXIS2_PLACEMENT_3D('',#15949,#8299,#8300);
#7025=AXIS2_PLACEMENT_3D('',#15951,#8301,#8302);
#7026=AXIS2_PLACEMENT_3D('',#15952,#8303,#8304);
#7027=AXIS2_PLACEMENT_3D('',#15954,#8305,#8306);
#7028=AXIS2_PLACEMENT_3D('',#15955,#8307,#8308);
#7029=AXIS2_PLACEMENT_3D('',#15957,#8309,#8310);
#7030=AXIS2_PLACEMENT_3D('',#15959,#8312,#8313);
#7031=AXIS2_PLACEMENT_3D('',#15961,#8314,#8315);
#7032=AXIS2_PLACEMENT_3D('',#15963,#8316,#8317);
#7033=AXIS2_PLACEMENT_3D('',#15964,#8318,#8319);
#7034=AXIS2_PLACEMENT_3D('',#15967,#8321,#8322);
#7035=AXIS2_PLACEMENT_3D('',#15968,#8323,#8324);
#7036=AXIS2_PLACEMENT_3D('',#15969,#8325,#8326);
#7037=AXIS2_PLACEMENT_3D('',#15971,#8328,#8329);
#7038=AXIS2_PLACEMENT_3D('',#15972,#8330,#8331);
#7039=AXIS2_PLACEMENT_3D('',#15973,#8332,#8333);
#7040=AXIS2_PLACEMENT_3D('',#15975,#8334,#8335);
#7041=AXIS2_PLACEMENT_3D('',#15978,#8337,#8338);
#7042=AXIS2_PLACEMENT_3D('',#15979,#8339,#8340);
#7043=AXIS2_PLACEMENT_3D('',#15981,#8341,#8342);
#7044=AXIS2_PLACEMENT_3D('',#15984,#8344,#8345);
#7045=AXIS2_PLACEMENT_3D('',#15985,#8346,#8347);
#7046=AXIS2_PLACEMENT_3D('',#15986,#8348,#8349);
#7047=AXIS2_PLACEMENT_3D('',#15987,#8350,#8351);
#7048=AXIS2_PLACEMENT_3D('',#15988,#8352,#8353);
#7049=AXIS2_PLACEMENT_3D('',#15990,#8354,#8355);
#7050=AXIS2_PLACEMENT_3D('',#15993,#8357,#8358);
#7051=AXIS2_PLACEMENT_3D('',#15994,#8359,#8360);
#7052=AXIS2_PLACEMENT_3D('',#15996,#8361,#8362);
#7053=AXIS2_PLACEMENT_3D('',#15999,#8364,#8365);
#7054=AXIS2_PLACEMENT_3D('',#16000,#8366,#8367);
#7055=AXIS2_PLACEMENT_3D('',#16001,#8368,#8369);
#7056=AXIS2_PLACEMENT_3D('',#16002,#8370,#8371);
#7057=AXIS2_PLACEMENT_3D('',#16003,#8372,#8373);
#7058=AXIS2_PLACEMENT_3D('',#16012,#8378,#8379);
#7059=AXIS2_PLACEMENT_3D('',#16021,#8384,#8385);
#7060=AXIS2_PLACEMENT_3D('',#16022,#8386,#8387);
#7061=AXIS2_PLACEMENT_3D('',#16023,#8388,#8389);
#7062=AXIS2_PLACEMENT_3D('',#16024,#8390,#8391);
#7063=AXIS2_PLACEMENT_3D('',#16025,#8392,#8393);
#7064=AXIS2_PLACEMENT_3D('',#16026,#8394,#8395);
#7065=AXIS2_PLACEMENT_3D('',#16027,#8396,#8397);
#7066=AXIS2_PLACEMENT_3D('',#16028,#8398,#8399);
#7067=AXIS2_PLACEMENT_3D('',#16029,#8400,#8401);
#7068=AXIS2_PLACEMENT_3D('',#16030,#8402,#8403);
#7069=AXIS2_PLACEMENT_3D('',#16032,#8404,#8405);
#7070=AXIS2_PLACEMENT_3D('',#16035,#8407,#8408);
#7071=AXIS2_PLACEMENT_3D('',#16036,#8409,#8410);
#7072=AXIS2_PLACEMENT_3D('',#16038,#8411,#8412);
#7073=AXIS2_PLACEMENT_3D('',#16041,#8414,#8415);
#7074=AXIS2_PLACEMENT_3D('',#16042,#8416,#8417);
#7075=AXIS2_PLACEMENT_3D('',#16043,#8418,#8419);
#7076=AXIS2_PLACEMENT_3D('',#16044,#8420,#8421);
#7077=AXIS2_PLACEMENT_3D('',#16045,#8422,#8423);
#7078=AXIS2_PLACEMENT_3D('',#16057,#8425,#8426);
#7079=AXIS2_PLACEMENT_3D('',#16062,#8427,#8428);
#7080=AXIS2_PLACEMENT_3D('',#16087,#8430,#8431);
#7081=AXIS2_PLACEMENT_3D('',#16111,#8433,#8434);
#7082=AXIS2_PLACEMENT_3D('',#16136,#8436,#8437);
#7083=AXIS2_PLACEMENT_3D('',#16161,#8439,#8440);
#7084=AXIS2_PLACEMENT_3D('',#16185,#8442,#8443);
#7085=AXIS2_PLACEMENT_3D('',#16209,#8445,#8446);
#7086=AXIS2_PLACEMENT_3D('',#16234,#8448,#8449);
#7087=AXIS2_PLACEMENT_3D('',#16253,#8451,#8452);
#7088=AXIS2_PLACEMENT_3D('',#16261,#8453,#8454);
#7089=AXIS2_PLACEMENT_3D('',#16309,#8456,#8457);
#7090=AXIS2_PLACEMENT_3D('',#16357,#8459,#8460);
#7091=AXIS2_PLACEMENT_3D('',#16405,#8462,#8463);
#7092=AXIS2_PLACEMENT_3D('',#16459,#8465,#8466);
#7093=AXIS2_PLACEMENT_3D('',#16507,#8468,#8469);
#7094=AXIS2_PLACEMENT_3D('',#16555,#8471,#8472);
#7095=AXIS2_PLACEMENT_3D('',#16557,#8473,#8474);
#7096=AXIS2_PLACEMENT_3D('',#16641,#8476,#8477);
#7097=AXIS2_PLACEMENT_3D('',#17206,#8478,#8479);
#7098=AXIS2_PLACEMENT_3D('',#17227,#8480,#8481);
#7099=AXIS2_PLACEMENT_3D('',#17228,#8482,#8483);
#7100=AXIS2_PLACEMENT_3D('',#17237,#8488,#8489);
#7101=AXIS2_PLACEMENT_3D('',#17243,#8493,#8494);
#7102=AXIS2_PLACEMENT_3D('',#17249,#8498,#8499);
#7103=AXIS2_PLACEMENT_3D('',#17255,#8503,#8504);
#7104=AXIS2_PLACEMENT_3D('',#17261,#8508,#8509);
#7105=AXIS2_PLACEMENT_3D('',#17264,#8512,#8513);
#7106=AXIS2_PLACEMENT_3D('',#17570,#8514,#8515);
#7107=AXIS2_PLACEMENT_3D('',#17571,#8516,#8517);
#7108=AXIS2_PLACEMENT_3D('',#17573,#8518,#8519);
#7109=AXIS2_PLACEMENT_3D('',#17575,#8520,#8521);
#7110=AXIS2_PLACEMENT_3D('',#17576,#8522,#8523);
#7111=AXIS2_PLACEMENT_3D('',#17578,#8524,#8525);
#7112=AXIS2_PLACEMENT_3D('',#17580,#8527,#8528);
#7113=AXIS2_PLACEMENT_3D('',#17581,#8529,#8530);
#7114=AXIS2_PLACEMENT_3D('',#17583,#8531,#8532);
#7115=AXIS2_PLACEMENT_3D('',#17584,#8533,#8534);
#7116=AXIS2_PLACEMENT_3D('',#17586,#8536,#8537);
#7117=AXIS2_PLACEMENT_3D('',#17587,#8538,#8539);
#7118=AXIS2_PLACEMENT_3D('',#17588,#8540,#8541);
#7119=AXIS2_PLACEMENT_3D('',#17604,#8543,#8544);
#7120=AXIS2_PLACEMENT_3D('',#17612,#8545,#8546);
#7121=AXIS2_PLACEMENT_3D('',#17660,#8548,#8549);
#7122=AXIS2_PLACEMENT_3D('',#17708,#8551,#8552);
#7123=AXIS2_PLACEMENT_3D('',#17759,#8554,#8555);
#7124=AXIS2_PLACEMENT_3D('',#17807,#8557,#8558);
#7125=AXIS2_PLACEMENT_3D('',#17855,#8560,#8561);
#7126=AXIS2_PLACEMENT_3D('',#17903,#8563,#8564);
#7127=AXIS2_PLACEMENT_3D('',#17957,#8566,#8567);
#7128=AXIS2_PLACEMENT_3D('',#18005,#8569,#8570);
#7129=AXIS2_PLACEMENT_3D('',#18053,#8572,#8573);
#7130=AXIS2_PLACEMENT_3D('',#18107,#8575,#8576);
#7131=AXIS2_PLACEMENT_3D('',#18155,#8578,#8579);
#7132=AXIS2_PLACEMENT_3D('',#18203,#8581,#8582);
#7133=AXIS2_PLACEMENT_3D('',#18218,#8584,#8585);
#7134=AXIS2_PLACEMENT_3D('',#18227,#8586,#8587);
#7135=AXIS2_PLACEMENT_3D('',#18251,#8589,#8590);
#7136=AXIS2_PLACEMENT_3D('',#18275,#8592,#8593);
#7137=AXIS2_PLACEMENT_3D('',#18300,#8595,#8596);
#7138=AXIS2_PLACEMENT_3D('',#18325,#8598,#8599);
#7139=AXIS2_PLACEMENT_3D('',#18349,#8601,#8602);
#7140=AXIS2_PLACEMENT_3D('',#18374,#8604,#8605);
#7141=AXIS2_PLACEMENT_3D('',#18399,#8607,#8608);
#7142=AXIS2_PLACEMENT_3D('',#18423,#8610,#8611);
#7143=AXIS2_PLACEMENT_3D('',#18447,#8613,#8614);
#7144=AXIS2_PLACEMENT_3D('',#18472,#8616,#8617);
#7145=AXIS2_PLACEMENT_3D('',#18497,#8619,#8620);
#7146=AXIS2_PLACEMENT_3D('',#18521,#8622,#8623);
#7147=AXIS2_PLACEMENT_3D('',#18746,#8624,#8625);
#7148=AXIS2_PLACEMENT_3D('',#18813,#8627,#8628);
#7149=AXIS2_PLACEMENT_3D('',#19276,#8629,#8630);
#7150=AXIS2_PLACEMENT_3D('',#19287,#8631,#8632);
#7151=AXIS2_PLACEMENT_3D('',#19749,#8633,#8634);
#7152=AXIS2_PLACEMENT_3D('',#19750,#8635,#8636);
#7153=AXIS2_PLACEMENT_3D('',#19759,#8641,#8642);
#7154=AXIS2_PLACEMENT_3D('',#19765,#8646,#8647);
#7155=AXIS2_PLACEMENT_3D('',#19771,#8651,#8652);
#7156=AXIS2_PLACEMENT_3D('',#19777,#8656,#8657);
#7157=AXIS2_PLACEMENT_3D('',#19783,#8661,#8662);
#7158=AXIS2_PLACEMENT_3D('',#19786,#8665,#8666);
#7159=AXIS2_PLACEMENT_3D('',#19787,#8667,#8668);
#7160=AXIS2_PLACEMENT_3D('',#19789,#8669,#8670);
#7161=AXIS2_PLACEMENT_3D('',#19790,#8671,#8672);
#7162=AXIS2_PLACEMENT_3D('',#19793,#8674,#8675);
#7163=AXIS2_PLACEMENT_3D('',#19794,#8676,#8677);
#7164=AXIS2_PLACEMENT_3D('',#19795,#8678,#8679);
#7165=AXIS2_PLACEMENT_3D('',#19796,#8680,#8681);
#7166=AXIS2_PLACEMENT_3D('',#19797,#8682,#8683);
#7167=AXIS2_PLACEMENT_3D('',#19798,#8684,#8685);
#7168=AXIS2_PLACEMENT_3D('',#19799,#8686,#8687);
#7169=AXIS2_PLACEMENT_3D('',#19800,#8688,#8689);
#7170=AXIS2_PLACEMENT_3D('',#19801,#8690,#8691);
#7171=AXIS2_PLACEMENT_3D('',#19802,#8692,#8693);
#7172=AXIS2_PLACEMENT_3D('',#19803,#8694,#8695);
#7173=AXIS2_PLACEMENT_3D('',#19804,#8696,#8697);
#7174=AXIS2_PLACEMENT_3D('',#19805,#8698,#8699);
#7175=AXIS2_PLACEMENT_3D('',#19806,#8700,#8701);
#7176=AXIS2_PLACEMENT_3D('',#19807,#8702,#8703);
#7177=AXIS2_PLACEMENT_3D('',#19808,#8704,#8705);
#7178=AXIS2_PLACEMENT_3D('',#19809,#8706,#8707);
#7179=AXIS2_PLACEMENT_3D('',#19810,#8708,#8709);
#7180=AXIS2_PLACEMENT_3D('',#19811,#8710,#8711);
#7181=AXIS2_PLACEMENT_3D('',#19812,#8712,#8713);
#7182=AXIS2_PLACEMENT_3D('',#19813,#8714,#8715);
#7183=AXIS2_PLACEMENT_3D('',#19814,#8716,#8717);
#7184=AXIS2_PLACEMENT_3D('',#19815,#8718,#8719);
#7185=AXIS2_PLACEMENT_3D('',#19816,#8720,#8721);
#7186=AXIS2_PLACEMENT_3D('',#19817,#8722,#8723);
#7187=AXIS2_PLACEMENT_3D('',#19818,#8724,#8725);
#7188=AXIS2_PLACEMENT_3D('',#19819,#8726,#8727);
#7189=AXIS2_PLACEMENT_3D('',#19820,#8728,#8729);
#7190=AXIS2_PLACEMENT_3D('',#19821,#8730,#8731);
#7191=DIRECTION('axis',(0.,0.,1.));
#7192=DIRECTION('refdir',(1.,0.,0.));
#7193=DIRECTION('axis',(0.,0.,1.));
#7194=DIRECTION('refdir',(1.,0.,0.));
#7195=DIRECTION('center_axis',(0.,0.,-1.));
#7196=DIRECTION('ref_axis',(1.,0.,0.));
#7197=DIRECTION('center_axis',(0.,0.,-1.));
#7198=DIRECTION('ref_axis',(1.,0.,0.));
#7199=DIRECTION('center_axis',(0.,0.,-1.));
#7200=DIRECTION('ref_axis',(1.,0.,0.));
#7201=DIRECTION('center_axis',(0.,0.,-1.));
#7202=DIRECTION('ref_axis',(1.,0.,0.));
#7203=DIRECTION('center_axis',(0.,0.,-1.));
#7204=DIRECTION('ref_axis',(1.,0.,0.));
#7205=DIRECTION('',(0.,0.,-1.));
#7206=DIRECTION('center_axis',(0.,0.,-1.));
#7207=DIRECTION('ref_axis',(1.,0.,0.));
#7208=DIRECTION('',(0.,0.,-1.));
#7209=DIRECTION('center_axis',(0.,0.,1.));
#7210=DIRECTION('ref_axis',(1.,0.,0.));
#7211=DIRECTION('center_axis',(0.,0.,-1.));
#7212=DIRECTION('ref_axis',(1.,0.,0.));
#7213=DIRECTION('center_axis',(0.,0.,-1.));
#7214=DIRECTION('ref_axis',(1.,0.,0.));
#7215=DIRECTION('center_axis',(0.,0.,-1.));
#7216=DIRECTION('ref_axis',(1.,0.,0.));
#7217=DIRECTION('center_axis',(0.,0.,-1.));
#7218=DIRECTION('ref_axis',(1.,0.,0.));
#7219=DIRECTION('center_axis',(0.,0.,-1.));
#7220=DIRECTION('ref_axis',(1.,0.,0.));
#7221=DIRECTION('',(0.,0.,-1.));
#7222=DIRECTION('center_axis',(0.,0.,-1.));
#7223=DIRECTION('ref_axis',(1.,0.,0.));
#7224=DIRECTION('',(0.,0.,-1.));
#7225=DIRECTION('center_axis',(0.,0.,1.));
#7226=DIRECTION('ref_axis',(1.,0.,0.));
#7227=DIRECTION('center_axis',(0.,0.,-1.));
#7228=DIRECTION('ref_axis',(1.,0.,0.));
#7229=DIRECTION('center_axis',(0.,0.,-1.));
#7230=DIRECTION('ref_axis',(1.,0.,0.));
#7231=DIRECTION('',(0.,0.,-1.));
#7232=DIRECTION('center_axis',(0.,0.,1.));
#7233=DIRECTION('ref_axis',(1.,0.,0.));
#7234=DIRECTION('center_axis',(0.,0.,-1.));
#7235=DIRECTION('ref_axis',(1.,0.,0.));
#7236=DIRECTION('center_axis',(0.,0.,-1.));
#7237=DIRECTION('ref_axis',(1.,0.,0.));
#7238=DIRECTION('',(0.,0.,-1.));
#7239=DIRECTION('center_axis',(0.,0.,1.));
#7240=DIRECTION('ref_axis',(1.,0.,0.));
#7241=DIRECTION('center_axis',(0.,0.,-1.));
#7242=DIRECTION('ref_axis',(1.,0.,0.));
#7243=DIRECTION('center_axis',(0.,0.,-1.));
#7244=DIRECTION('ref_axis',(1.,0.,0.));
#7245=DIRECTION('',(0.,0.,-1.));
#7246=DIRECTION('center_axis',(0.,0.,1.));
#7247=DIRECTION('ref_axis',(1.,0.,0.));
#7248=DIRECTION('center_axis',(0.,0.,-1.));
#7249=DIRECTION('ref_axis',(1.,0.,0.));
#7250=DIRECTION('center_axis',(0.,0.,-1.));
#7251=DIRECTION('ref_axis',(1.,0.,0.));
#7252=DIRECTION('',(0.,0.,-1.));
#7253=DIRECTION('center_axis',(0.,0.,1.));
#7254=DIRECTION('ref_axis',(1.,0.,0.));
#7255=DIRECTION('center_axis',(0.,-1.,0.));
#7256=DIRECTION('ref_axis',(-1.,0.,0.));
#7257=DIRECTION('',(-1.,0.,0.));
#7258=DIRECTION('',(0.,0.,-1.));
#7259=DIRECTION('',(1.,0.,0.));
#7260=DIRECTION('',(0.,0.,-1.));
#7261=DIRECTION('center_axis',(1.,0.,0.));
#7262=DIRECTION('ref_axis',(0.,-1.,0.));
#7263=DIRECTION('',(0.,-1.,0.));
#7264=DIRECTION('',(0.,0.,-1.));
#7265=DIRECTION('',(0.,1.,0.));
#7266=DIRECTION('center_axis',(0.,1.,0.));
#7267=DIRECTION('ref_axis',(1.,0.,0.));
#7268=DIRECTION('',(1.,0.,0.));
#7269=DIRECTION('',(0.,0.,-1.));
#7270=DIRECTION('',(-1.,0.,0.));
#7271=DIRECTION('center_axis',(-1.,0.,0.));
#7272=DIRECTION('ref_axis',(0.,1.,0.));
#7273=DIRECTION('',(0.,1.,0.));
#7274=DIRECTION('',(0.,-1.,0.));
#7275=DIRECTION('center_axis',(0.,-1.,0.));
#7276=DIRECTION('ref_axis',(-1.,0.,0.));
#7277=DIRECTION('',(-1.,0.,0.));
#7278=DIRECTION('',(0.,0.,-1.));
#7279=DIRECTION('',(1.,0.,0.));
#7280=DIRECTION('',(0.,0.,-1.));
#7281=DIRECTION('center_axis',(1.,0.,0.));
#7282=DIRECTION('ref_axis',(0.,-1.,0.));
#7283=DIRECTION('',(0.,-1.,0.));
#7284=DIRECTION('',(0.,0.,-1.));
#7285=DIRECTION('',(0.,1.,0.));
#7286=DIRECTION('center_axis',(0.,1.,0.));
#7287=DIRECTION('ref_axis',(1.,0.,0.));
#7288=DIRECTION('',(1.,0.,0.));
#7289=DIRECTION('',(0.,0.,-1.));
#7290=DIRECTION('',(-1.,0.,0.));
#7291=DIRECTION('center_axis',(-1.,0.,0.));
#7292=DIRECTION('ref_axis',(0.,1.,0.));
#7293=DIRECTION('',(0.,1.,0.));
#7294=DIRECTION('',(0.,-1.,0.));
#7295=DIRECTION('center_axis',(0.,1.,0.));
#7296=DIRECTION('ref_axis',(-1.,0.,0.));
#7297=DIRECTION('',(1.,0.,0.));
#7298=DIRECTION('',(0.,0.,-1.));
#7299=DIRECTION('',(-1.,0.,0.));
#7300=DIRECTION('',(0.,0.,1.));
#7301=DIRECTION('center_axis',(0.,-1.,0.));
#7302=DIRECTION('ref_axis',(1.,0.,0.));
#7303=DIRECTION('',(-1.,0.,0.));
#7304=DIRECTION('',(0.,0.,1.));
#7305=DIRECTION('',(1.,0.,0.));
#7306=DIRECTION('',(0.,0.,1.));
#7307=DIRECTION('center_axis',(0.,0.,1.));
#7308=DIRECTION('ref_axis',(1.,0.,0.));
#7309=DIRECTION('',(0.,1.,0.));
#7310=DIRECTION('',(0.,1.,0.));
#7311=DIRECTION('center_axis',(0.,0.,1.));
#7312=DIRECTION('ref_axis',(1.,0.,0.));
#7313=DIRECTION('',(0.,1.,0.));
#7314=DIRECTION('',(1.,0.,0.));
#7315=DIRECTION('',(0.,1.,0.));
#7316=DIRECTION('center_axis',(0.,0.,1.));
#7317=DIRECTION('ref_axis',(1.,0.,0.));
#7318=DIRECTION('',(0.,1.,0.));
#7319=DIRECTION('',(1.,0.,0.));
#7320=DIRECTION('',(0.,1.,0.));
#7321=DIRECTION('center_axis',(0.,1.,0.));
#7322=DIRECTION('ref_axis',(-1.,0.,0.));
#7323=DIRECTION('',(0.,0.,-1.));
#7324=DIRECTION('',(-1.,0.,0.));
#7325=DIRECTION('',(0.,0.,1.));
#7326=DIRECTION('center_axis',(0.,-1.,0.));
#7327=DIRECTION('ref_axis',(1.,0.,0.));
#7328=DIRECTION('',(-1.,0.,0.));
#7329=DIRECTION('',(0.,0.,1.));
#7330=DIRECTION('',(1.,0.,0.));
#7331=DIRECTION('',(0.,0.,1.));
#7332=DIRECTION('center_axis',(0.,0.,1.));
#7333=DIRECTION('ref_axis',(1.,0.,0.));
#7334=DIRECTION('',(0.,1.,0.));
#7335=DIRECTION('',(0.,1.,0.));
#7336=DIRECTION('center_axis',(0.,0.,1.));
#7337=DIRECTION('ref_axis',(1.,0.,0.));
#7338=DIRECTION('',(0.,1.,0.));
#7339=DIRECTION('',(-1.,0.,0.));
#7340=DIRECTION('',(0.,1.,0.));
#7341=DIRECTION('center_axis',(0.,1.,0.));
#7342=DIRECTION('ref_axis',(-1.,0.,0.));
#7343=DIRECTION('',(1.,0.,0.));
#7344=DIRECTION('',(0.,0.,-1.));
#7345=DIRECTION('',(0.,0.,-1.));
#7346=DIRECTION('center_axis',(1.,0.,0.));
#7347=DIRECTION('ref_axis',(0.,1.,0.));
#7348=DIRECTION('',(0.,1.,0.));
#7349=DIRECTION('',(0.,0.,1.));
#7350=DIRECTION('center_axis',(0.,-1.,0.));
#7351=DIRECTION('ref_axis',(1.,0.,0.));
#7352=DIRECTION('',(-1.,0.,0.));
#7353=DIRECTION('',(0.,0.,1.));
#7354=DIRECTION('center_axis',(-1.,0.,0.));
#7355=DIRECTION('ref_axis',(0.,-1.,0.));
#7356=DIRECTION('',(0.,1.,0.));
#7357=DIRECTION('center_axis',(0.,0.,1.));
#7358=DIRECTION('ref_axis',(1.,0.,0.));
#7359=DIRECTION('axis',(0.,0.,1.));
#7360=DIRECTION('refdir',(1.,0.,0.));
#7361=DIRECTION('center_axis',(0.,0.,-1.));
#7362=DIRECTION('ref_axis',(1.,0.,0.));
#7363=DIRECTION('',(0.,0.,-1.));
#7364=DIRECTION('center_axis',(0.,0.,1.));
#7365=DIRECTION('ref_axis',(1.,0.,0.));
#7366=DIRECTION('',(0.,0.,-1.));
#7367=DIRECTION('center_axis',(0.,0.,1.));
#7368=DIRECTION('ref_axis',(1.,0.,0.));
#7369=DIRECTION('center_axis',(0.,0.,-1.));
#7370=DIRECTION('ref_axis',(1.,0.,0.));
#7371=DIRECTION('',(0.,0.,-1.));
#7372=DIRECTION('center_axis',(0.,0.,-1.));
#7373=DIRECTION('ref_axis',(1.,0.,0.));
#7374=DIRECTION('',(0.,0.,-1.));
#7375=DIRECTION('center_axis',(0.,0.,-1.));
#7376=DIRECTION('ref_axis',(1.,0.,0.));
#7377=DIRECTION('',(0.,0.,-1.));
#7378=DIRECTION('center_axis',(0.,0.,-1.));
#7379=DIRECTION('ref_axis',(1.,0.,0.));
#7380=DIRECTION('',(0.,0.,-1.));
#7381=DIRECTION('center_axis',(0.,0.,-1.));
#7382=DIRECTION('ref_axis',(1.,0.,0.));
#7383=DIRECTION('',(0.,0.,-1.));
#7384=DIRECTION('center_axis',(0.,0.,-1.));
#7385=DIRECTION('ref_axis',(1.,0.,0.));
#7386=DIRECTION('',(0.,0.,-1.));
#7387=DIRECTION('center_axis',(0.,0.,-1.));
#7388=DIRECTION('ref_axis',(1.,0.,0.));
#7389=DIRECTION('',(0.,0.,-1.));
#7390=DIRECTION('center_axis',(0.,0.,-1.));
#7391=DIRECTION('ref_axis',(1.,0.,0.));
#7392=DIRECTION('',(0.,0.,-1.));
#7393=DIRECTION('center_axis',(0.,0.,-1.));
#7394=DIRECTION('ref_axis',(1.,0.,0.));
#7395=DIRECTION('',(0.,0.,-1.));
#7396=DIRECTION('center_axis',(0.,0.,-1.));
#7397=DIRECTION('ref_axis',(1.,0.,0.));
#7398=DIRECTION('',(0.,0.,-1.));
#7399=DIRECTION('center_axis',(0.,0.,-1.));
#7400=DIRECTION('ref_axis',(1.,0.,0.));
#7401=DIRECTION('',(0.,0.,-1.));
#7402=DIRECTION('center_axis',(0.,0.,-1.));
#7403=DIRECTION('ref_axis',(1.,0.,0.));
#7404=DIRECTION('',(0.,0.,-1.));
#7405=DIRECTION('center_axis',(0.,0.,-1.));
#7406=DIRECTION('ref_axis',(1.,0.,0.));
#7407=DIRECTION('',(0.,0.,-1.));
#7408=DIRECTION('center_axis',(0.,0.,-1.));
#7409=DIRECTION('ref_axis',(0.938438541741608,-0.345446238036955,0.));
#7410=DIRECTION('',(0.,0.,-1.));
#7411=DIRECTION('center_axis',(0.,0.,-1.));
#7412=DIRECTION('ref_axis',(1.,0.,0.));
#7413=DIRECTION('center_axis',(0.,0.,-1.));
#7414=DIRECTION('ref_axis',(0.0179644034331435,0.999838627084037,0.));
#7415=DIRECTION('',(1.22464679914735E-16,-8.74945686026681E-30,-1.));
#7416=DIRECTION('center_axis',(0.,0.,1.));
#7417=DIRECTION('ref_axis',(1.,-7.13222724178225E-14,0.));
#7418=DIRECTION('center_axis',(0.,0.,-1.));
#7419=DIRECTION('ref_axis',(1.,-7.13222724178225E-14,0.));
#7420=DIRECTION('',(1.22464679914735E-16,-8.74945686026681E-30,-1.));
#7421=DIRECTION('center_axis',(0.,0.,-1.));
#7422=DIRECTION('ref_axis',(1.,-7.13222724178225E-14,0.));
#7423=DIRECTION('',(1.22464679914735E-16,-8.74945686026681E-30,-1.));
#7424=DIRECTION('center_axis',(0.,0.,-1.));
#7425=DIRECTION('ref_axis',(1.,-7.13222724178225E-14,0.));
#7426=DIRECTION('',(1.22464679914735E-16,-8.74945686026681E-30,-1.));
#7427=DIRECTION('center_axis',(0.,0.,-1.));
#7428=DIRECTION('ref_axis',(1.,-7.13222724178225E-14,0.));
#7429=DIRECTION('',(1.22464679914735E-16,-8.74945686026681E-30,-1.));
#7430=DIRECTION('center_axis',(0.,0.,-1.));
#7431=DIRECTION('ref_axis',(1.,-7.13222724178225E-14,0.));
#7432=DIRECTION('',(1.22464679914735E-16,-8.74945686026681E-30,-1.));
#7433=DIRECTION('center_axis',(0.,0.,-1.));
#7434=DIRECTION('ref_axis',(1.,-7.13222724178225E-14,0.));
#7435=DIRECTION('',(1.22464679914735E-16,-8.74945686026681E-30,-1.));
#7436=DIRECTION('center_axis',(0.,0.,-1.));
#7437=DIRECTION('ref_axis',(1.,-7.13222724178225E-14,0.));
#7438=DIRECTION('',(1.22464679914735E-16,-8.74945686026681E-30,-1.));
#7439=DIRECTION('center_axis',(0.,0.,-1.));
#7440=DIRECTION('ref_axis',(1.,-7.13222724178225E-14,0.));
#7441=DIRECTION('',(1.22464679914735E-16,-8.74945686026681E-30,-1.));
#7442=DIRECTION('center_axis',(0.,0.,-1.));
#7443=DIRECTION('ref_axis',(1.,-7.13222724178225E-14,0.));
#7444=DIRECTION('',(1.22464679914735E-16,-8.74945686026681E-30,-1.));
#7445=DIRECTION('center_axis',(0.,0.,-1.));
#7446=DIRECTION('ref_axis',(1.,-7.13222724178225E-14,0.));
#7447=DIRECTION('',(1.22464679914735E-16,-8.74945686026681E-30,-1.));
#7448=DIRECTION('center_axis',(0.,0.,-1.));
#7449=DIRECTION('ref_axis',(1.,-7.13222724178225E-14,0.));
#7450=DIRECTION('',(1.22464679914735E-16,-8.74945686026681E-30,-1.));
#7451=DIRECTION('center_axis',(0.,0.,-1.));
#7452=DIRECTION('ref_axis',(1.,-7.13222724178225E-14,0.));
#7453=DIRECTION('',(1.22464679914735E-16,-8.74945686026681E-30,-1.));
#7454=DIRECTION('center_axis',(0.,0.,-1.));
#7455=DIRECTION('ref_axis',(1.,-7.13222724178225E-14,0.));
#7456=DIRECTION('',(1.22464679914735E-16,-8.74945686026681E-30,-1.));
#7457=DIRECTION('center_axis',(0.,0.,-1.));
#7458=DIRECTION('ref_axis',(1.,-7.13222724178225E-14,0.));
#7459=DIRECTION('',(1.22464679914735E-16,-8.74945686026681E-30,-1.));
#7460=DIRECTION('center_axis',(0.,0.,-1.));
#7461=DIRECTION('ref_axis',(-0.609341687186091,-0.792907755200571,0.));
#7462=DIRECTION('',(1.22464679914735E-16,-8.74945686026681E-30,-1.));
#7463=DIRECTION('center_axis',(0.,0.,-1.));
#7464=DIRECTION('ref_axis',(1.,-7.13222724178225E-14,0.));
#7465=DIRECTION('center_axis',(0.,0.,-1.));
#7466=DIRECTION('ref_axis',(1.,0.,0.));
#7467=DIRECTION('',(0.,0.,-1.));
#7468=DIRECTION('center_axis',(0.,0.,1.));
#7469=DIRECTION('ref_axis',(1.,0.,0.));
#7470=DIRECTION('',(0.,0.,-1.));
#7471=DIRECTION('center_axis',(0.,0.,1.));
#7472=DIRECTION('ref_axis',(1.,0.,0.));
#7473=DIRECTION('center_axis',(0.,0.,-1.));
#7474=DIRECTION('ref_axis',(1.,0.,0.));
#7475=DIRECTION('',(0.,0.,-1.));
#7476=DIRECTION('center_axis',(0.,0.,-1.));
#7477=DIRECTION('ref_axis',(1.,0.,0.));
#7478=DIRECTION('',(0.,0.,-1.));
#7479=DIRECTION('center_axis',(0.,0.,-1.));
#7480=DIRECTION('ref_axis',(1.,0.,0.));
#7481=DIRECTION('',(0.,0.,-1.));
#7482=DIRECTION('center_axis',(0.,0.,-1.));
#7483=DIRECTION('ref_axis',(1.,0.,0.));
#7484=DIRECTION('',(0.,0.,-1.));
#7485=DIRECTION('center_axis',(0.,0.,-1.));
#7486=DIRECTION('ref_axis',(1.,0.,0.));
#7487=DIRECTION('',(0.,0.,-1.));
#7488=DIRECTION('center_axis',(0.,0.,-1.));
#7489=DIRECTION('ref_axis',(1.,0.,0.));
#7490=DIRECTION('',(0.,0.,-1.));
#7491=DIRECTION('center_axis',(0.,0.,-1.));
#7492=DIRECTION('ref_axis',(1.,0.,0.));
#7493=DIRECTION('',(0.,0.,-1.));
#7494=DIRECTION('center_axis',(0.,0.,-1.));
#7495=DIRECTION('ref_axis',(1.,0.,0.));
#7496=DIRECTION('',(0.,0.,-1.));
#7497=DIRECTION('center_axis',(0.,0.,-1.));
#7498=DIRECTION('ref_axis',(1.,0.,0.));
#7499=DIRECTION('',(0.,0.,-1.));
#7500=DIRECTION('center_axis',(0.,0.,-1.));
#7501=DIRECTION('ref_axis',(1.,0.,0.));
#7502=DIRECTION('',(0.,0.,-1.));
#7503=DIRECTION('center_axis',(0.,0.,-1.));
#7504=DIRECTION('ref_axis',(1.,0.,0.));
#7505=DIRECTION('',(0.,0.,-1.));
#7506=DIRECTION('center_axis',(0.,0.,-1.));
#7507=DIRECTION('ref_axis',(1.,0.,0.));
#7508=DIRECTION('',(0.,0.,-1.));
#7509=DIRECTION('center_axis',(0.,0.,-1.));
#7510=DIRECTION('ref_axis',(1.,0.,0.));
#7511=DIRECTION('',(0.,0.,-1.));
#7512=DIRECTION('center_axis',(0.,0.,-1.));
#7513=DIRECTION('ref_axis',(0.93843855055824,-0.345446214085711,0.));
#7514=DIRECTION('',(0.,0.,-1.));
#7515=DIRECTION('center_axis',(0.,0.,-1.));
#7516=DIRECTION('ref_axis',(1.,0.,0.));
#7517=DIRECTION('center_axis',(0.,0.,-1.));
#7518=DIRECTION('ref_axis',(0.0179644055674462,0.999838627045689,0.));
#7519=DIRECTION('',(1.22464679914735E-16,-8.74945686026681E-30,-1.));
#7520=DIRECTION('center_axis',(0.,0.,1.));
#7521=DIRECTION('ref_axis',(1.,-7.13222724178225E-14,0.));
#7522=DIRECTION('center_axis',(0.,0.,-1.));
#7523=DIRECTION('ref_axis',(1.,-7.13222724178225E-14,0.));
#7524=DIRECTION('',(1.22464679914735E-16,-8.74945686026681E-30,-1.));
#7525=DIRECTION('center_axis',(0.,0.,-1.));
#7526=DIRECTION('ref_axis',(1.,-7.13222724178225E-14,0.));
#7527=DIRECTION('',(1.22464679914735E-16,-8.74945686026681E-30,-1.));
#7528=DIRECTION('center_axis',(0.,0.,-1.));
#7529=DIRECTION('ref_axis',(1.,-7.13222724178225E-14,0.));
#7530=DIRECTION('',(1.22464679914735E-16,-8.74945686026681E-30,-1.));
#7531=DIRECTION('center_axis',(0.,0.,-1.));
#7532=DIRECTION('ref_axis',(1.,-7.13222724178225E-14,0.));
#7533=DIRECTION('',(1.22464679914735E-16,-8.74945686026681E-30,-1.));
#7534=DIRECTION('center_axis',(0.,0.,-1.));
#7535=DIRECTION('ref_axis',(1.,-7.13222724178225E-14,0.));
#7536=DIRECTION('',(1.22464679914735E-16,-8.74945686026681E-30,-1.));
#7537=DIRECTION('center_axis',(0.,0.,-1.));
#7538=DIRECTION('ref_axis',(1.,-7.13222724178225E-14,0.));
#7539=DIRECTION('',(1.22464679914735E-16,-8.74945686026681E-30,-1.));
#7540=DIRECTION('center_axis',(0.,0.,-1.));
#7541=DIRECTION('ref_axis',(1.,-7.13222724178225E-14,0.));
#7542=DIRECTION('',(1.22464679914735E-16,-8.74945686026681E-30,-1.));
#7543=DIRECTION('center_axis',(0.,0.,-1.));
#7544=DIRECTION('ref_axis',(1.,-7.13222724178225E-14,0.));
#7545=DIRECTION('',(1.22464679914735E-16,-8.74945686026681E-30,-1.));
#7546=DIRECTION('center_axis',(0.,0.,-1.));
#7547=DIRECTION('ref_axis',(1.,-7.13222724178225E-14,0.));
#7548=DIRECTION('',(1.22464679914735E-16,-8.74945686026681E-30,-1.));
#7549=DIRECTION('center_axis',(0.,0.,-1.));
#7550=DIRECTION('ref_axis',(1.,-7.13222724178225E-14,0.));
#7551=DIRECTION('',(1.22464679914735E-16,-8.74945686026681E-30,-1.));
#7552=DIRECTION('center_axis',(0.,0.,-1.));
#7553=DIRECTION('ref_axis',(1.,-7.13222724178225E-14,0.));
#7554=DIRECTION('',(1.22464679914735E-16,-8.74945686026681E-30,-1.));
#7555=DIRECTION('center_axis',(0.,0.,-1.));
#7556=DIRECTION('ref_axis',(1.,-7.13222724178225E-14,0.));
#7557=DIRECTION('',(1.22464679914735E-16,-8.74945686026681E-30,-1.));
#7558=DIRECTION('center_axis',(0.,0.,-1.));
#7559=DIRECTION('ref_axis',(1.,-7.13222724178225E-14,0.));
#7560=DIRECTION('',(1.22464679914735E-16,-8.74945686026681E-30,-1.));
#7561=DIRECTION('center_axis',(0.,0.,-1.));
#7562=DIRECTION('ref_axis',(1.,-7.13222724178225E-14,0.));
#7563=DIRECTION('',(1.22464679914735E-16,-8.74945686026681E-30,-1.));
#7564=DIRECTION('center_axis',(0.,0.,-1.));
#7565=DIRECTION('ref_axis',(-0.609341710614343,-0.792907737196193,0.));
#7566=DIRECTION('',(1.22464679914735E-16,-8.74945686026681E-30,-1.));
#7567=DIRECTION('center_axis',(0.,0.,-1.));
#7568=DIRECTION('ref_axis',(1.,-7.13222724178225E-14,0.));
#7569=DIRECTION('center_axis',(0.,0.,1.));
#7570=DIRECTION('ref_axis',(1.,0.,0.));
#7571=DIRECTION('center_axis',(0.,0.,-1.));
#7572=DIRECTION('ref_axis',(1.,-7.13222724178225E-14,0.));
#7573=DIRECTION('center_axis',(0.,0.,-1.));
#7574=DIRECTION('ref_axis',(1.,0.,0.));
#7575=DIRECTION('center_axis',(0.,0.,1.));
#7576=DIRECTION('ref_axis',(1.,0.,0.));
#7577=DIRECTION('center_axis',(0.,0.,-1.));
#7578=DIRECTION('ref_axis',(1.,-7.13222724178225E-14,0.));
#7579=DIRECTION('center_axis',(0.,0.,-1.));
#7580=DIRECTION('ref_axis',(1.,0.,0.));
#7581=DIRECTION('center_axis',(0.,0.,-1.));
#7582=DIRECTION('ref_axis',(1.,0.,0.));
#7583=DIRECTION('center_axis',(0.,0.,-1.));
#7584=DIRECTION('ref_axis',(1.,0.,0.));
#7585=DIRECTION('center_axis',(0.,-1.,0.));
#7586=DIRECTION('ref_axis',(0.,0.,1.));
#7587=DIRECTION('center_axis',(0.,-1.,0.));
#7588=DIRECTION('ref_axis',(0.,0.,1.));
#7589=DIRECTION('',(0.,-1.,0.));
#7590=DIRECTION('center_axis',(0.,1.,0.));
#7591=DIRECTION('ref_axis',(0.,0.,1.));
#7592=DIRECTION('center_axis',(0.,-1.,0.));
#7593=DIRECTION('ref_axis',(0.,0.,1.));
#7594=DIRECTION('center_axis',(0.,-1.,0.));
#7595=DIRECTION('ref_axis',(0.,0.,1.));
#7596=DIRECTION('',(0.,-1.,0.));
#7597=DIRECTION('center_axis',(0.,1.,0.));
#7598=DIRECTION('ref_axis',(0.,0.,1.));
#7599=DIRECTION('center_axis',(0.,-1.,0.));
#7600=DIRECTION('ref_axis',(0.,0.,1.));
#7601=DIRECTION('center_axis',(0.,-1.,0.));
#7602=DIRECTION('ref_axis',(0.,0.,1.));
#7603=DIRECTION('',(0.,-1.,0.));
#7604=DIRECTION('center_axis',(0.,1.,0.));
#7605=DIRECTION('ref_axis',(0.,0.,1.));
#7606=DIRECTION('center_axis',(-1.,0.,0.));
#7607=DIRECTION('ref_axis',(0.,-1.,0.));
#7608=DIRECTION('',(0.,-1.,0.));
#7609=DIRECTION('',(0.,0.,1.));
#7610=DIRECTION('',(0.,-1.,0.));
#7611=DIRECTION('',(0.,0.,1.));
#7612=DIRECTION('center_axis',(1.,0.,0.));
#7613=DIRECTION('ref_axis',(0.,1.,0.));
#7614=DIRECTION('',(0.,1.,0.));
#7615=DIRECTION('',(0.,0.,1.));
#7616=DIRECTION('',(0.,1.,0.));
#7617=DIRECTION('',(0.,0.,1.));
#7618=DIRECTION('center_axis',(0.,0.,1.));
#7619=DIRECTION('ref_axis',(1.,0.,0.));
#7620=DIRECTION('',(-1.,0.,0.));
#7621=DIRECTION('',(1.,0.,0.));
#7622=DIRECTION('center_axis',(0.,0.,1.));
#7623=DIRECTION('ref_axis',(1.,0.,0.));
#7624=DIRECTION('',(1.,0.,0.));
#7625=DIRECTION('',(0.,-1.,0.));
#7626=DIRECTION('',(-1.,0.,0.));
#7627=DIRECTION('center_axis',(0.,0.,1.));
#7628=DIRECTION('ref_axis',(1.,0.,0.));
#7629=DIRECTION('',(-1.,0.,0.));
#7630=DIRECTION('',(0.,1.,0.));
#7631=DIRECTION('',(1.,0.,0.));
#7632=DIRECTION('center_axis',(0.,-1.,0.));
#7633=DIRECTION('ref_axis',(1.,0.,0.));
#7634=DIRECTION('',(1.,0.,0.));
#7635=DIRECTION('',(0.,0.,1.));
#7636=DIRECTION('',(1.,0.,0.));
#7637=DIRECTION('',(0.,0.,1.));
#7638=DIRECTION('center_axis',(-1.,0.,0.));
#7639=DIRECTION('ref_axis',(0.,-1.,0.));
#7640=DIRECTION('',(0.,-1.,0.));
#7641=DIRECTION('',(0.,0.,1.));
#7642=DIRECTION('',(0.,-1.,0.));
#7643=DIRECTION('center_axis',(1.,0.,0.));
#7644=DIRECTION('ref_axis',(0.,1.,0.));
#7645=DIRECTION('',(0.,1.,0.));
#7646=DIRECTION('',(0.,1.,0.));
#7647=DIRECTION('',(0.,0.,1.));
#7648=DIRECTION('center_axis',(0.,0.,1.));
#7649=DIRECTION('ref_axis',(1.,0.,0.));
#7650=DIRECTION('',(-1.,0.,0.));
#7651=DIRECTION('center_axis',(0.,0.,1.));
#7652=DIRECTION('ref_axis',(1.,0.,0.));
#7653=DIRECTION('',(-1.,0.,0.));
#7654=DIRECTION('',(0.,1.,0.));
#7655=DIRECTION('',(1.,0.,0.));
#7656=DIRECTION('',(0.,1.,0.));
#7657=DIRECTION('',(-1.,0.,0.));
#7658=DIRECTION('',(0.,-1.,0.));
#7659=DIRECTION('',(1.,0.,0.));
#7660=DIRECTION('',(0.,-1.,0.));
#7661=DIRECTION('',(-1.,0.,0.));
#7662=DIRECTION('',(1.,0.,0.));
#7663=DIRECTION('',(0.,1.,0.));
#7664=DIRECTION('',(-1.,0.,0.));
#7665=DIRECTION('',(0.,-1.,0.));
#7666=DIRECTION('',(1.,0.,0.));
#7667=DIRECTION('',(0.,1.,0.));
#7668=DIRECTION('',(-1.,0.,0.));
#7669=DIRECTION('',(0.,-1.,0.));
#7670=DIRECTION('center_axis',(0.,1.,0.));
#7671=DIRECTION('ref_axis',(-1.,0.,0.));
#7672=DIRECTION('',(0.,0.,1.));
#7673=DIRECTION('',(0.,0.,1.));
#7674=DIRECTION('center_axis',(1.,0.,0.));
#7675=DIRECTION('ref_axis',(0.,1.,0.));
#7676=DIRECTION('',(0.,0.,1.));
#7677=DIRECTION('center_axis',(-1.,0.,0.));
#7678=DIRECTION('ref_axis',(0.,-1.,0.));
#7679=DIRECTION('',(0.,0.,1.));
#7680=DIRECTION('center_axis',(0.,-1.,0.));
#7681=DIRECTION('ref_axis',(1.,0.,0.));
#7682=DIRECTION('',(0.,0.,1.));
#7683=DIRECTION('',(1.,0.,0.));
#7684=DIRECTION('',(0.,0.,-1.));
#7685=DIRECTION('',(-1.,0.,0.));
#7686=DIRECTION('',(0.,0.,1.));
#7687=DIRECTION('',(1.,0.,0.));
#7688=DIRECTION('',(0.,0.,1.));
#7689=DIRECTION('center_axis',(0.,-1.,0.));
#7690=DIRECTION('ref_axis',(-1.,0.,0.));
#7691=DIRECTION('',(-1.,0.,0.));
#7692=DIRECTION('',(0.,0.,-1.));
#7693=DIRECTION('',(0.,0.,-1.));
#7694=DIRECTION('center_axis',(1.,0.,0.));
#7695=DIRECTION('ref_axis',(0.,-1.,0.));
#7696=DIRECTION('',(0.,-1.,0.));
#7697=DIRECTION('',(0.,0.,-1.));
#7698=DIRECTION('center_axis',(0.,1.,0.));
#7699=DIRECTION('ref_axis',(1.,0.,0.));
#7700=DIRECTION('',(1.,0.,0.));
#7701=DIRECTION('',(0.,0.,-1.));
#7702=DIRECTION('center_axis',(-1.,0.,0.));
#7703=DIRECTION('ref_axis',(0.,1.,0.));
#7704=DIRECTION('',(0.,1.,0.));
#7705=DIRECTION('center_axis',(0.,-1.,0.));
#7706=DIRECTION('ref_axis',(-1.,0.,0.));
#7707=DIRECTION('',(-1.,0.,0.));
#7708=DIRECTION('',(0.,0.,-1.));
#7709=DIRECTION('',(0.,0.,-1.));
#7710=DIRECTION('center_axis',(1.,0.,0.));
#7711=DIRECTION('ref_axis',(0.,-1.,0.));
#7712=DIRECTION('',(0.,-1.,0.));
#7713=DIRECTION('',(0.,0.,-1.));
#7714=DIRECTION('center_axis',(0.,1.,0.));
#7715=DIRECTION('ref_axis',(1.,0.,0.));
#7716=DIRECTION('',(1.,0.,0.));
#7717=DIRECTION('',(0.,0.,-1.));
#7718=DIRECTION('center_axis',(-1.,0.,0.));
#7719=DIRECTION('ref_axis',(0.,1.,0.));
#7720=DIRECTION('',(0.,1.,0.));
#7721=DIRECTION('center_axis',(-1.,0.,0.));
#7722=DIRECTION('ref_axis',(0.,-1.,0.));
#7723=DIRECTION('',(0.,0.,-1.));
#7724=DIRECTION('',(0.,1.,0.));
#7725=DIRECTION('',(0.,-1.,0.));
#7726=DIRECTION('',(0.,0.,1.));
#7727=DIRECTION('',(0.,-1.,0.));
#7728=DIRECTION('',(0.,0.,1.));
#7729=DIRECTION('',(0.,-1.,0.));
#7730=DIRECTION('center_axis',(0.,0.,1.));
#7731=DIRECTION('ref_axis',(1.,0.,0.));
#7732=DIRECTION('',(0.,1.,0.));
#7733=DIRECTION('',(1.,0.,0.));
#7734=DIRECTION('center_axis',(0.,0.,1.));
#7735=DIRECTION('ref_axis',(1.,0.,0.));
#7736=DIRECTION('',(1.,0.,0.));
#7737=DIRECTION('',(-1.,0.,0.));
#7738=DIRECTION('',(0.,1.,0.));
#7739=DIRECTION('center_axis',(0.,1.,0.));
#7740=DIRECTION('ref_axis',(-1.,0.,0.));
#7741=DIRECTION('',(-1.,0.,0.));
#7742=DIRECTION('',(0.,0.,1.));
#7743=DIRECTION('center_axis',(1.,0.,0.));
#7744=DIRECTION('ref_axis',(0.,1.,0.));
#7745=DIRECTION('',(0.,0.,1.));
#7746=DIRECTION('',(0.,1.,0.));
#7747=DIRECTION('',(0.,0.,1.));
#7748=DIRECTION('',(0.,-1.,0.));
#7749=DIRECTION('center_axis',(0.,-1.,0.));
#7750=DIRECTION('ref_axis',(1.,0.,0.));
#7751=DIRECTION('',(1.,0.,0.));
#7752=DIRECTION('center_axis',(0.,0.,1.));
#7753=DIRECTION('ref_axis',(1.,0.,0.));
#7754=DIRECTION('center_axis',(0.,0.,1.));
#7755=DIRECTION('ref_axis',(1.,0.,0.));
#7756=DIRECTION('',(-1.,0.,0.));
#7757=DIRECTION('',(0.,-1.,0.));
#7758=DIRECTION('center_axis',(0.,0.,1.));
#7759=DIRECTION('ref_axis',(1.,0.,0.));
#7760=DIRECTION('',(0.,1.,0.));
#7761=DIRECTION('',(-1.,0.,0.));
#7762=DIRECTION('center_axis',(0.,1.,0.));
#7763=DIRECTION('ref_axis',(-1.,0.,0.));
#7764=DIRECTION('',(0.,0.,1.));
#7765=DIRECTION('',(0.,0.,1.));
#7766=DIRECTION('center_axis',(1.,0.,0.));
#7767=DIRECTION('ref_axis',(0.,1.,0.));
#7768=DIRECTION('center_axis',(-1.,0.,0.));
#7769=DIRECTION('ref_axis',(0.,-1.,0.));
#7770=DIRECTION('axis',(0.,0.,1.));
#7771=DIRECTION('refdir',(1.,0.,0.));
#7772=DIRECTION('center_axis',(0.,0.,-1.));
#7773=DIRECTION('ref_axis',(-0.346960385471041,0.937879784894517,0.));
#7774=DIRECTION('',(0.,0.,-1.));
#7775=DIRECTION('center_axis',(0.,0.,-1.));
#7776=DIRECTION('ref_axis',(1.,0.,0.));
#7777=DIRECTION('center_axis',(0.,0.,-1.));
#7778=DIRECTION('ref_axis',(1.,0.,0.));
#7779=DIRECTION('',(0.,0.,-1.));
#7780=DIRECTION('center_axis',(0.,0.,-1.));
#7781=DIRECTION('ref_axis',(1.,0.,0.));
#7782=DIRECTION('',(0.,0.,-1.));
#7783=DIRECTION('center_axis',(0.,0.,-1.));
#7784=DIRECTION('ref_axis',(1.,0.,0.));
#7785=DIRECTION('',(0.,0.,-1.));
#7786=DIRECTION('center_axis',(0.,0.,-1.));
#7787=DIRECTION('ref_axis',(1.,0.,0.));
#7788=DIRECTION('',(0.,0.,-1.));
#7789=DIRECTION('center_axis',(0.,0.,-1.));
#7790=DIRECTION('ref_axis',(1.,0.,0.));
#7791=DIRECTION('',(0.,0.,-1.));
#7792=DIRECTION('center_axis',(0.,0.,-1.));
#7793=DIRECTION('ref_axis',(1.,0.,0.));
#7794=DIRECTION('',(0.,0.,-1.));
#7795=DIRECTION('center_axis',(0.,0.,-1.));
#7796=DIRECTION('ref_axis',(1.,0.,0.));
#7797=DIRECTION('',(0.,0.,-1.));
#7798=DIRECTION('center_axis',(0.,0.,-1.));
#7799=DIRECTION('ref_axis',(1.,0.,0.));
#7800=DIRECTION('',(0.,0.,-1.));
#7801=DIRECTION('center_axis',(0.,0.,-1.));
#7802=DIRECTION('ref_axis',(0.937992883095123,-0.346654512826386,0.));
#7803=DIRECTION('',(0.,0.,-1.));
#7804=DIRECTION('center_axis',(0.,0.,-1.));
#7805=DIRECTION('ref_axis',(1.,0.,0.));
#7806=DIRECTION('center_axis',(0.,0.,-1.));
#7807=DIRECTION('ref_axis',(1.,-3.75673318890569E-14,0.));
#7808=DIRECTION('',(1.22464679914735E-16,-4.6156688728706E-30,-1.));
#7809=DIRECTION('center_axis',(0.,0.,1.));
#7810=DIRECTION('ref_axis',(1.,-3.75673318890569E-14,0.));
#7811=DIRECTION('center_axis',(0.,0.,-1.));
#7812=DIRECTION('ref_axis',(1.,-3.75673318890569E-14,0.));
#7813=DIRECTION('',(1.22464679914735E-16,-4.6156688728706E-30,-1.));
#7814=DIRECTION('center_axis',(0.,0.,-1.));
#7815=DIRECTION('ref_axis',(1.,-3.75673318890569E-14,0.));
#7816=DIRECTION('',(1.22464679914735E-16,-4.6156688728706E-30,-1.));
#7817=DIRECTION('center_axis',(0.,0.,-1.));
#7818=DIRECTION('ref_axis',(1.,-3.75673318890569E-14,0.));
#7819=DIRECTION('',(1.22464679914735E-16,-4.6156688728706E-30,-1.));
#7820=DIRECTION('center_axis',(0.,0.,-1.));
#7821=DIRECTION('ref_axis',(1.,-3.75673318890569E-14,0.));
#7822=DIRECTION('',(1.22464679914735E-16,-4.6156688728706E-30,-1.));
#7823=DIRECTION('center_axis',(0.,0.,-1.));
#7824=DIRECTION('ref_axis',(1.,-3.75673318890569E-14,0.));
#7825=DIRECTION('',(1.22464679914735E-16,-4.6156688728706E-30,-1.));
#7826=DIRECTION('center_axis',(0.,0.,-1.));
#7827=DIRECTION('ref_axis',(1.,-3.75673318890569E-14,0.));
#7828=DIRECTION('',(1.22464679914735E-16,-4.6156688728706E-30,-1.));
#7829=DIRECTION('center_axis',(0.,0.,-1.));
#7830=DIRECTION('ref_axis',(1.,-3.75673318890569E-14,0.));
#7831=DIRECTION('',(1.22464679914735E-16,-4.6156688728706E-30,-1.));
#7832=DIRECTION('center_axis',(0.,0.,-1.));
#7833=DIRECTION('ref_axis',(1.,-3.75673318890569E-14,0.));
#7834=DIRECTION('',(1.22464679914735E-16,-4.6156688728706E-30,-1.));
#7835=DIRECTION('center_axis',(0.,0.,-1.));
#7836=DIRECTION('ref_axis',(-0.609232734071224,-0.792991472675527,0.));
#7837=DIRECTION('',(1.22464679914735E-16,-4.6156688728706E-30,-1.));
#7838=DIRECTION('center_axis',(0.,0.,-1.));
#7839=DIRECTION('ref_axis',(1.,-3.75673318890569E-14,0.));
#7840=DIRECTION('center_axis',(0.,0.,-1.));
#7841=DIRECTION('ref_axis',(0.275637355817,0.961261695938319,0.));
#7842=DIRECTION('center_axis',(0.,0.,-1.));
#7843=DIRECTION('ref_axis',(0.275637355817,0.961261695938319,0.));
#7844=DIRECTION('',(0.,0.,-1.));
#7845=DIRECTION('center_axis',(0.,0.,1.));
#7846=DIRECTION('ref_axis',(0.275637355817,0.961261695938319,0.));
#7847=DIRECTION('',(0.,0.,-1.));
#7848=DIRECTION('center_axis',(0.,0.,-1.));
#7849=DIRECTION('ref_axis',(-0.961261693884661,-0.275637362978957,0.));
#7850=DIRECTION('center_axis',(0.,0.,-1.));
#7851=DIRECTION('ref_axis',(-0.275637355816999,0.961261695938319,0.));
#7852=DIRECTION('',(0.,0.,-1.));
#7853=DIRECTION('center_axis',(0.,0.,1.));
#7854=DIRECTION('ref_axis',(-0.275637355816999,0.961261695938319,0.));
#7855=DIRECTION('center_axis',(0.,0.,-1.));
#7856=DIRECTION('ref_axis',(0.275637355816998,0.961261695938319,0.));
#7857=DIRECTION('center_axis',(0.,0.,1.));
#7858=DIRECTION('ref_axis',(0.275637355816998,0.961261695938319,0.));
#7859=DIRECTION('',(0.,0.,-1.));
#7860=DIRECTION('center_axis',(0.,0.,-1.));
#7861=DIRECTION('ref_axis',(0.275637355816998,0.961261695938319,0.));
#7862=DIRECTION('center_axis',(0.,0.,-1.));
#7863=DIRECTION('ref_axis',(-0.275637355817,-0.961261695938319,0.));
#7864=DIRECTION('center_axis',(0.,0.,-1.));
#7865=DIRECTION('ref_axis',(-0.275637355817,-0.961261695938319,0.));
#7866=DIRECTION('center_axis',(0.,0.,1.));
#7867=DIRECTION('ref_axis',(-0.275637355817,-0.961261695938319,0.));
#7868=DIRECTION('center_axis',(0.,0.,-1.));
#7869=DIRECTION('ref_axis',(1.,-3.75673318890569E-14,0.));
#7870=DIRECTION('center_axis',(0.,0.,1.));
#7871=DIRECTION('ref_axis',(1.,0.,0.));
#7872=DIRECTION('center_axis',(0.,0.,1.));
#7873=DIRECTION('ref_axis',(1.,0.,0.));
#7874=DIRECTION('center_axis',(0.,0.,-1.));
#7875=DIRECTION('ref_axis',(1.,0.,0.));
#7876=DIRECTION('center_axis',(0.,0.,-1.));
#7877=DIRECTION('ref_axis',(1.,0.,0.));
#7878=DIRECTION('center_axis',(0.,0.,-1.));
#7879=DIRECTION('ref_axis',(1.,0.,0.));
#7880=DIRECTION('',(0.,0.,-1.));
#7881=DIRECTION('center_axis',(0.,0.,1.));
#7882=DIRECTION('ref_axis',(1.,0.,0.));
#7883=DIRECTION('center_axis',(0.,0.,-1.));
#7884=DIRECTION('ref_axis',(1.,0.,0.));
#7885=DIRECTION('center_axis',(0.,0.,-1.));
#7886=DIRECTION('ref_axis',(1.,0.,0.));
#7887=DIRECTION('',(0.,0.,-1.));
#7888=DIRECTION('center_axis',(0.,0.,1.));
#7889=DIRECTION('ref_axis',(1.,0.,0.));
#7890=DIRECTION('center_axis',(0.,0.,-1.));
#7891=DIRECTION('ref_axis',(1.,0.,0.));
#7892=DIRECTION('center_axis',(0.,0.,-1.));
#7893=DIRECTION('ref_axis',(1.,0.,0.));
#7894=DIRECTION('',(0.,0.,-1.));
#7895=DIRECTION('center_axis',(0.,0.,1.));
#7896=DIRECTION('ref_axis',(1.,0.,0.));
#7897=DIRECTION('center_axis',(0.,0.,1.));
#7898=DIRECTION('ref_axis',(1.,0.,0.));
#7899=DIRECTION('',(0.,0.,-1.));
#7900=DIRECTION('center_axis',(0.,0.,-1.));
#7901=DIRECTION('ref_axis',(1.,0.,0.));
#7902=DIRECTION('center_axis',(0.,0.,1.));
#7903=DIRECTION('ref_axis',(1.,0.,0.));
#7904=DIRECTION('',(0.,0.,1.));
#7905=DIRECTION('center_axis',(0.,0.,1.));
#7906=DIRECTION('ref_axis',(1.,0.,0.));
#7907=DIRECTION('',(0.,0.,1.));
#7908=DIRECTION('center_axis',(0.,0.,1.));
#7909=DIRECTION('ref_axis',(1.,0.,0.));
#7910=DIRECTION('center_axis',(0.,0.,1.));
#7911=DIRECTION('ref_axis',(1.,0.,0.));
#7912=DIRECTION('',(0.,-1.,0.));
#7913=DIRECTION('',(-1.,0.,0.));
#7914=DIRECTION('center_axis',(0.,0.,1.));
#7915=DIRECTION('ref_axis',(0.,1.,0.));
#7916=DIRECTION('',(1.,0.,0.));
#7917=DIRECTION('center_axis',(0.,0.,1.));
#7918=DIRECTION('ref_axis',(1.,0.,0.));
#7919=DIRECTION('',(1.,0.,0.));
#7920=DIRECTION('center_axis',(0.,0.,1.));
#7921=DIRECTION('ref_axis',(0.,-1.,0.));
#7922=DIRECTION('',(-1.,0.,0.));
#7923=DIRECTION('',(0.,1.,0.));
#7924=DIRECTION('center_axis',(1.,0.,0.));
#7925=DIRECTION('ref_axis',(0.,1.,0.));
#7926=DIRECTION('',(0.,0.,1.));
#7927=DIRECTION('',(0.,1.,0.));
#7928=DIRECTION('center_axis',(-1.,0.,0.));
#7929=DIRECTION('ref_axis',(0.,-1.,0.));
#7930=DIRECTION('',(0.,0.,-1.));
#7931=DIRECTION('',(0.,-1.,0.));
#7932=DIRECTION('center_axis',(0.,1.,0.));
#7933=DIRECTION('ref_axis',(-1.,0.,0.));
#7934=DIRECTION('',(-1.,0.,0.));
#7935=DIRECTION('',(0.,0.,1.));
#7936=DIRECTION('center_axis',(0.,0.,1.));
#7937=DIRECTION('ref_axis',(1.,0.,0.));
#7938=DIRECTION('',(-1.,0.,0.));
#7939=DIRECTION('center_axis',(0.,0.,1.));
#7940=DIRECTION('ref_axis',(0.,-1.,0.));
#7941=DIRECTION('',(1.,0.,0.));
#7942=DIRECTION('center_axis',(0.,0.,1.));
#7943=DIRECTION('ref_axis',(1.,0.,0.));
#7944=DIRECTION('',(1.,0.,0.));
#7945=DIRECTION('center_axis',(0.,0.,1.));
#7946=DIRECTION('ref_axis',(0.,1.,0.));
#7947=DIRECTION('center_axis',(0.,0.,1.));
#7948=DIRECTION('ref_axis',(1.,0.,0.));
#7949=DIRECTION('',(0.,0.,-1.));
#7950=DIRECTION('',(0.,0.,1.));
#7951=DIRECTION('center_axis',(0.,1.,0.));
#7952=DIRECTION('ref_axis',(-1.,0.,0.));
#7953=DIRECTION('',(0.,0.,1.));
#7954=DIRECTION('center_axis',(0.,-1.,0.));
#7955=DIRECTION('ref_axis',(1.,0.,0.));
#7956=DIRECTION('',(0.,0.,1.));
#7957=DIRECTION('center_axis',(0.,0.,1.));
#7958=DIRECTION('ref_axis',(0.,-1.,0.));
#7959=DIRECTION('',(0.,0.,1.));
#7960=DIRECTION('center_axis',(0.,-1.,0.));
#7961=DIRECTION('ref_axis',(1.,0.,0.));
#7962=DIRECTION('center_axis',(0.,0.,1.));
#7963=DIRECTION('ref_axis',(0.,1.,0.));
#7964=DIRECTION('axis',(0.,0.,1.));
#7965=DIRECTION('refdir',(1.,0.,0.));
#7966=DIRECTION('center_axis',(0.,0.,1.));
#7967=DIRECTION('ref_axis',(1.,0.,0.));
#7968=DIRECTION('',(0.,-1.,0.));
#7969=DIRECTION('',(1.,0.,0.));
#7970=DIRECTION('',(0.,1.,0.));
#7971=DIRECTION('',(-1.,0.,0.));
#7972=DIRECTION('center_axis',(0.,1.,0.));
#7973=DIRECTION('ref_axis',(-9.25185853854298E-17,0.,-1.));
#7974=DIRECTION('center_axis',(0.,1.,0.));
#7975=DIRECTION('ref_axis',(-9.25185853854298E-17,0.,-1.));
#7976=DIRECTION('',(0.,1.,0.));
#7977=DIRECTION('center_axis',(0.,-1.,0.));
#7978=DIRECTION('ref_axis',(-9.25185853854298E-17,0.,-1.));
#7979=DIRECTION('center_axis',(0.,0.,-1.));
#7980=DIRECTION('ref_axis',(-1.,0.,0.));
#7981=DIRECTION('',(-1.,0.,0.));
#7982=DIRECTION('',(0.,1.,0.));
#7983=DIRECTION('',(1.,0.,0.));
#7984=DIRECTION('center_axis',(0.,1.,0.));
#7985=DIRECTION('ref_axis',(9.25185853854298E-17,0.,1.));
#7986=DIRECTION('center_axis',(0.,1.,0.));
#7987=DIRECTION('ref_axis',(9.25185853854298E-17,0.,1.));
#7988=DIRECTION('center_axis',(0.,-1.,0.));
#7989=DIRECTION('ref_axis',(9.25185853854298E-17,0.,1.));
#7990=DIRECTION('center_axis',(0.,0.,1.));
#7991=DIRECTION('ref_axis',(1.,0.,0.));
#7992=DIRECTION('',(1.,0.,0.));
#7993=DIRECTION('',(0.,1.,0.));
#7994=DIRECTION('',(1.,0.,0.));
#7995=DIRECTION('',(0.,-1.,0.));
#7996=DIRECTION('center_axis',(0.,0.,1.));
#7997=DIRECTION('ref_axis',(1.,0.,0.));
#7998=DIRECTION('',(-1.,0.,0.));
#7999=DIRECTION('',(0.,-1.,0.));
#8000=DIRECTION('',(-1.,0.,0.));
#8001=DIRECTION('',(0.,1.,0.));
#8002=DIRECTION('center_axis',(0.,1.,0.));
#8003=DIRECTION('ref_axis',(-1.,0.,0.));
#8004=DIRECTION('',(0.,0.,1.));
#8005=DIRECTION('',(-1.,0.,0.));
#8006=DIRECTION('',(0.,0.,1.));
#8007=DIRECTION('center_axis',(1.,0.,0.));
#8008=DIRECTION('ref_axis',(0.,1.,0.));
#8009=DIRECTION('',(0.,-1.,0.));
#8010=DIRECTION('',(0.,1.,0.));
#8011=DIRECTION('',(0.,0.,1.));
#8012=DIRECTION('center_axis',(0.,-1.,0.));
#8013=DIRECTION('ref_axis',(1.,0.,0.));
#8014=DIRECTION('',(1.,0.,0.));
#8015=DIRECTION('',(0.,0.,1.));
#8016=DIRECTION('center_axis',(-1.,0.,0.));
#8017=DIRECTION('ref_axis',(0.,-1.,0.));
#8018=DIRECTION('',(0.,1.,0.));
#8019=DIRECTION('',(0.,-1.,0.));
#8020=DIRECTION('center_axis',(0.,0.,1.));
#8021=DIRECTION('ref_axis',(1.,0.,0.));
#8022=DIRECTION('center_axis',(0.,0.,1.));
#8023=DIRECTION('ref_axis',(1.,0.,0.));
#8024=DIRECTION('',(-1.,0.,0.));
#8025=DIRECTION('',(0.,-1.,0.));
#8026=DIRECTION('',(1.,0.,0.));
#8027=DIRECTION('center_axis',(0.,0.,1.));
#8028=DIRECTION('ref_axis',(1.,0.,0.));
#8029=DIRECTION('',(1.,0.,0.));
#8030=DIRECTION('',(0.,1.,0.));
#8031=DIRECTION('',(-1.,0.,0.));
#8032=DIRECTION('center_axis',(1.,0.,0.));
#8033=DIRECTION('ref_axis',(0.,1.,0.));
#8034=DIRECTION('',(0.,-1.,0.));
#8035=DIRECTION('',(0.,0.,1.));
#8036=DIRECTION('',(0.,0.,1.));
#8037=DIRECTION('center_axis',(-1.,0.,0.));
#8038=DIRECTION('ref_axis',(0.,-1.,0.));
#8039=DIRECTION('',(0.,1.,0.));
#8040=DIRECTION('',(0.,0.,1.));
#8041=DIRECTION('',(0.,0.,1.));
#8042=DIRECTION('center_axis',(0.,0.,1.));
#8043=DIRECTION('ref_axis',(1.,0.,0.));
#8044=DIRECTION('',(-1.,0.,0.));
#8045=DIRECTION('',(0.,-1.,0.));
#8046=DIRECTION('',(1.,0.,0.));
#8047=DIRECTION('center_axis',(0.,1.,0.));
#8048=DIRECTION('ref_axis',(-1.,0.,0.));
#8049=DIRECTION('',(-1.,0.,0.));
#8050=DIRECTION('',(0.,0.,1.));
#8051=DIRECTION('',(-1.,0.,0.));
#8052=DIRECTION('',(0.,0.,1.));
#8053=DIRECTION('center_axis',(1.,0.,0.));
#8054=DIRECTION('ref_axis',(0.,1.,0.));
#8055=DIRECTION('',(0.,1.,0.));
#8056=DIRECTION('',(0.,1.,0.));
#8057=DIRECTION('',(0.,0.,1.));
#8058=DIRECTION('center_axis',(0.,-1.,0.));
#8059=DIRECTION('ref_axis',(1.,0.,0.));
#8060=DIRECTION('',(1.,0.,0.));
#8061=DIRECTION('',(1.,0.,0.));
#8062=DIRECTION('',(0.,0.,1.));
#8063=DIRECTION('center_axis',(-1.,0.,0.));
#8064=DIRECTION('ref_axis',(0.,-1.,0.));
#8065=DIRECTION('',(0.,-1.,0.));
#8066=DIRECTION('center_axis',(0.,0.,1.));
#8067=DIRECTION('ref_axis',(1.,0.,0.));
#8068=DIRECTION('center_axis',(0.,0.,1.));
#8069=DIRECTION('ref_axis',(1.,0.,0.));
#8070=DIRECTION('axis',(0.,0.,1.));
#8071=DIRECTION('refdir',(1.,0.,0.));
#8072=DIRECTION('center_axis',(0.,0.,1.));
#8073=DIRECTION('ref_axis',(1.,0.,0.));
#8074=DIRECTION('center_axis',(0.,0.,1.));
#8075=DIRECTION('ref_axis',(1.,0.,0.));
#8076=DIRECTION('',(0.,0.,1.));
#8077=DIRECTION('center_axis',(0.,0.,1.));
#8078=DIRECTION('ref_axis',(1.,0.,0.));
#8079=DIRECTION('center_axis',(0.,0.,-1.));
#8080=DIRECTION('ref_axis',(-1.,0.,0.));
#8081=DIRECTION('center_axis',(0.,0.,-1.));
#8082=DIRECTION('ref_axis',(1.,0.,0.));
#8083=DIRECTION('center_axis',(0.,0.,1.));
#8084=DIRECTION('ref_axis',(1.,0.,0.));
#8085=DIRECTION('center_axis',(0.,0.,1.));
#8086=DIRECTION('ref_axis',(1.,0.,0.));
#8087=DIRECTION('center_axis',(0.,0.,1.));
#8088=DIRECTION('ref_axis',(1.,0.,0.));
#8089=DIRECTION('center_axis',(0.,0.,1.));
#8090=DIRECTION('ref_axis',(1.,0.,0.));
#8091=DIRECTION('',(0.,0.,-1.));
#8092=DIRECTION('center_axis',(0.,0.,1.));
#8093=DIRECTION('ref_axis',(1.,0.,0.));
#8094=DIRECTION('center_axis',(0.,0.,1.));
#8095=DIRECTION('ref_axis',(1.,0.,0.));
#8096=DIRECTION('center_axis',(0.,0.,1.));
#8097=DIRECTION('ref_axis',(1.,0.,0.));
#8098=DIRECTION('center_axis',(0.,0.,1.));
#8099=DIRECTION('ref_axis',(1.,0.,0.));
#8100=DIRECTION('',(0.,0.,-1.));
#8101=DIRECTION('center_axis',(0.,0.,1.));
#8102=DIRECTION('ref_axis',(1.,0.,0.));
#8103=DIRECTION('center_axis',(0.,0.,1.));
#8104=DIRECTION('ref_axis',(1.,0.,0.));
#8105=DIRECTION('center_axis',(0.,0.,1.));
#8106=DIRECTION('ref_axis',(1.,0.,0.));
#8107=DIRECTION('',(0.,0.,-1.));
#8108=DIRECTION('center_axis',(0.,0.,1.));
#8109=DIRECTION('ref_axis',(1.,0.,0.));
#8110=DIRECTION('axis',(0.,0.,1.));
#8111=DIRECTION('refdir',(1.,0.,0.));
#8112=DIRECTION('center_axis',(0.,0.,1.));
#8113=DIRECTION('ref_axis',(1.,0.,0.));
#8114=DIRECTION('center_axis',(0.,0.,1.));
#8115=DIRECTION('ref_axis',(1.,0.,0.));
#8116=DIRECTION('',(0.,0.,1.));
#8117=DIRECTION('center_axis',(0.,0.,1.));
#8118=DIRECTION('ref_axis',(1.,0.,0.));
#8119=DIRECTION('center_axis',(0.,0.,-1.));
#8120=DIRECTION('ref_axis',(-1.,0.,0.));
#8121=DIRECTION('center_axis',(0.,0.,-1.));
#8122=DIRECTION('ref_axis',(1.,0.,0.));
#8123=DIRECTION('center_axis',(0.,0.,1.));
#8124=DIRECTION('ref_axis',(1.,0.,0.));
#8125=DIRECTION('center_axis',(0.,0.,1.));
#8126=DIRECTION('ref_axis',(1.,0.,0.));
#8127=DIRECTION('center_axis',(0.,0.,1.));
#8128=DIRECTION('ref_axis',(1.,0.,0.));
#8129=DIRECTION('center_axis',(0.,0.,1.));
#8130=DIRECTION('ref_axis',(1.,0.,0.));
#8131=DIRECTION('',(0.,0.,-1.));
#8132=DIRECTION('center_axis',(0.,0.,1.));
#8133=DIRECTION('ref_axis',(1.,0.,0.));
#8134=DIRECTION('center_axis',(0.,0.,1.));
#8135=DIRECTION('ref_axis',(1.,0.,0.));
#8136=DIRECTION('center_axis',(0.,0.,1.));
#8137=DIRECTION('ref_axis',(1.,0.,0.));
#8138=DIRECTION('center_axis',(0.,0.,1.));
#8139=DIRECTION('ref_axis',(1.,0.,0.));
#8140=DIRECTION('',(0.,0.,-1.));
#8141=DIRECTION('center_axis',(0.,0.,1.));
#8142=DIRECTION('ref_axis',(1.,0.,0.));
#8143=DIRECTION('center_axis',(0.,0.,1.));
#8144=DIRECTION('ref_axis',(1.,0.,0.));
#8145=DIRECTION('center_axis',(0.,0.,1.));
#8146=DIRECTION('ref_axis',(1.,0.,0.));
#8147=DIRECTION('',(0.,0.,-1.));
#8148=DIRECTION('center_axis',(0.,0.,1.));
#8149=DIRECTION('ref_axis',(1.,0.,0.));
#8150=DIRECTION('axis',(0.,0.,1.));
#8151=DIRECTION('refdir',(1.,0.,0.));
#8152=DIRECTION('center_axis',(0.,0.,1.));
#8153=DIRECTION('ref_axis',(1.,0.,0.));
#8154=DIRECTION('center_axis',(0.,0.,-1.));
#8155=DIRECTION('ref_axis',(1.,0.,0.));
#8156=DIRECTION('',(0.,0.,-1.));
#8157=DIRECTION('center_axis',(0.,0.,-1.));
#8158=DIRECTION('ref_axis',(1.,0.,0.));
#8159=DIRECTION('center_axis',(0.,0.,1.));
#8160=DIRECTION('ref_axis',(1.,0.,0.));
#8161=DIRECTION('center_axis',(0.,0.,1.));
#8162=DIRECTION('ref_axis',(1.,0.,0.));
#8163=DIRECTION('',(0.,0.,-1.));
#8164=DIRECTION('center_axis',(0.,0.,1.));
#8165=DIRECTION('ref_axis',(1.,0.,0.));
#8166=DIRECTION('center_axis',(0.,0.,1.));
#8167=DIRECTION('ref_axis',(1.,0.,0.));
#8168=DIRECTION('center_axis',(0.,0.,1.));
#8169=DIRECTION('ref_axis',(1.,0.,0.));
#8170=DIRECTION('axis',(0.,0.,1.));
#8171=DIRECTION('refdir',(1.,0.,0.));
#8172=DIRECTION('center_axis',(-1.,0.,0.));
#8173=DIRECTION('ref_axis',(0.,1.,0.));
#8174=DIRECTION('',(0.,0.,1.));
#8175=DIRECTION('',(0.,-1.,0.));
#8176=DIRECTION('',(0.,0.,-1.));
#8177=DIRECTION('',(0.,1.,0.));
#8178=DIRECTION('center_axis',(1.,0.,0.));
#8179=DIRECTION('ref_axis',(0.,-1.,0.));
#8180=DIRECTION('',(0.,0.,-1.));
#8181=DIRECTION('',(0.,-1.,0.));
#8182=DIRECTION('',(0.,0.,1.));
#8183=DIRECTION('',(0.,1.,0.));
#8184=DIRECTION('center_axis',(0.,0.,1.));
#8185=DIRECTION('ref_axis',(1.,0.,0.));
#8186=DIRECTION('center_axis',(0.,0.,1.));
#8187=DIRECTION('ref_axis',(1.,0.,0.));
#8188=DIRECTION('center_axis',(0.,0.,-1.));
#8189=DIRECTION('ref_axis',(1.,0.,0.));
#8190=DIRECTION('center_axis',(0.,0.,1.));
#8191=DIRECTION('ref_axis',(6.12323399573677E-17,-1.,0.));
#8192=DIRECTION('center_axis',(0.,0.,-1.));
#8193=DIRECTION('ref_axis',(1.,0.,0.));
#8194=DIRECTION('center_axis',(0.,0.,1.));
#8195=DIRECTION('ref_axis',(6.12323399573677E-17,-1.,0.));
#8196=DIRECTION('center_axis',(0.,0.,1.));
#8197=DIRECTION('ref_axis',(1.,0.,0.));
#8198=DIRECTION('center_axis',(0.,0.,1.));
#8199=DIRECTION('ref_axis',(1.,0.,0.));
#8200=DIRECTION('axis',(0.,0.,1.));
#8201=DIRECTION('refdir',(1.,0.,0.));
#8202=DIRECTION('center_axis',(0.,0.,1.));
#8203=DIRECTION('ref_axis',(1.,0.,0.));
#8204=DIRECTION('center_axis',(0.,0.,-1.));
#8205=DIRECTION('ref_axis',(1.,0.,0.));
#8206=DIRECTION('',(0.,0.,-1.));
#8207=DIRECTION('center_axis',(0.,0.,-1.));
#8208=DIRECTION('ref_axis',(1.,0.,0.));
#8209=DIRECTION('center_axis',(0.,0.,1.));
#8210=DIRECTION('ref_axis',(1.,0.,0.));
#8211=DIRECTION('center_axis',(0.,0.,1.));
#8212=DIRECTION('ref_axis',(1.,0.,0.));
#8213=DIRECTION('',(0.,0.,-1.));
#8214=DIRECTION('center_axis',(0.,0.,1.));
#8215=DIRECTION('ref_axis',(1.,0.,0.));
#8216=DIRECTION('center_axis',(0.,0.,1.));
#8217=DIRECTION('ref_axis',(1.,0.,0.));
#8218=DIRECTION('center_axis',(0.,0.,1.));
#8219=DIRECTION('ref_axis',(1.,0.,0.));
#8220=DIRECTION('axis',(0.,0.,1.));
#8221=DIRECTION('refdir',(1.,0.,0.));
#8222=DIRECTION('center_axis',(0.,0.,1.));
#8223=DIRECTION('ref_axis',(1.,0.,0.));
#8224=DIRECTION('center_axis',(0.,0.,-1.));
#8225=DIRECTION('ref_axis',(1.,0.,0.));
#8226=DIRECTION('',(0.,0.,-1.));
#8227=DIRECTION('center_axis',(0.,0.,-1.));
#8228=DIRECTION('ref_axis',(1.,0.,0.));
#8229=DIRECTION('center_axis',(0.,0.,1.));
#8230=DIRECTION('ref_axis',(1.,0.,0.));
#8231=DIRECTION('center_axis',(0.,0.,1.));
#8232=DIRECTION('ref_axis',(1.,0.,0.));
#8233=DIRECTION('',(0.,0.,-1.));
#8234=DIRECTION('center_axis',(0.,0.,1.));
#8235=DIRECTION('ref_axis',(1.,0.,0.));
#8236=DIRECTION('center_axis',(0.,0.,1.));
#8237=DIRECTION('ref_axis',(1.,0.,0.));
#8238=DIRECTION('center_axis',(0.,0.,1.));
#8239=DIRECTION('ref_axis',(1.,0.,0.));
#8240=DIRECTION('axis',(0.,0.,1.));
#8241=DIRECTION('refdir',(1.,0.,0.));
#8242=DIRECTION('center_axis',(0.,0.,1.));
#8243=DIRECTION('ref_axis',(1.,0.,0.));
#8244=DIRECTION('center_axis',(0.,0.,-1.));
#8245=DIRECTION('ref_axis',(1.,0.,0.));
#8246=DIRECTION('',(0.,0.,-1.));
#8247=DIRECTION('center_axis',(0.,0.,-1.));
#8248=DIRECTION('ref_axis',(1.,0.,0.));
#8249=DIRECTION('center_axis',(0.,0.,1.));
#8250=DIRECTION('ref_axis',(1.,0.,0.));
#8251=DIRECTION('center_axis',(0.,0.,1.));
#8252=DIRECTION('ref_axis',(1.,0.,0.));
#8253=DIRECTION('',(0.,0.,-1.));
#8254=DIRECTION('center_axis',(0.,0.,1.));
#8255=DIRECTION('ref_axis',(1.,0.,0.));
#8256=DIRECTION('center_axis',(0.,0.,1.));
#8257=DIRECTION('ref_axis',(1.,0.,0.));
#8258=DIRECTION('center_axis',(0.,0.,1.));
#8259=DIRECTION('ref_axis',(1.,0.,0.));
#8260=DIRECTION('axis',(0.,0.,1.));
#8261=DIRECTION('refdir',(1.,0.,0.));
#8262=DIRECTION('center_axis',(-1.,0.,0.));
#8263=DIRECTION('ref_axis',(0.,1.,0.));
#8264=DIRECTION('',(0.,0.,1.));
#8265=DIRECTION('',(0.,-1.,0.));
#8266=DIRECTION('',(0.,0.,-1.));
#8267=DIRECTION('',(0.,1.,0.));
#8268=DIRECTION('center_axis',(1.,0.,0.));
#8269=DIRECTION('ref_axis',(0.,-1.,0.));
#8270=DIRECTION('',(0.,0.,-1.));
#8271=DIRECTION('',(0.,-1.,0.));
#8272=DIRECTION('',(0.,0.,1.));
#8273=DIRECTION('',(0.,1.,0.));
#8274=DIRECTION('center_axis',(0.,0.,1.));
#8275=DIRECTION('ref_axis',(1.,0.,0.));
#8276=DIRECTION('center_axis',(0.,0.,1.));
#8277=DIRECTION('ref_axis',(1.,0.,0.));
#8278=DIRECTION('center_axis',(0.,0.,-1.));
#8279=DIRECTION('ref_axis',(1.,0.,0.));
#8280=DIRECTION('center_axis',(0.,0.,1.));
#8281=DIRECTION('ref_axis',(6.12323399573677E-17,-1.,0.));
#8282=DIRECTION('center_axis',(0.,0.,-1.));
#8283=DIRECTION('ref_axis',(1.,0.,0.));
#8284=DIRECTION('center_axis',(0.,0.,1.));
#8285=DIRECTION('ref_axis',(6.12323399573677E-17,-1.,0.));
#8286=DIRECTION('center_axis',(0.,0.,1.));
#8287=DIRECTION('ref_axis',(1.,0.,0.));
#8288=DIRECTION('center_axis',(0.,0.,1.));
#8289=DIRECTION('ref_axis',(1.,0.,0.));
#8290=DIRECTION('axis',(0.,0.,1.));
#8291=DIRECTION('refdir',(1.,0.,0.));
#8292=DIRECTION('center_axis',(0.,0.,1.));
#8293=DIRECTION('ref_axis',(1.,0.,0.));
#8294=DIRECTION('center_axis',(0.,0.,1.));
#8295=DIRECTION('ref_axis',(1.,0.,0.));
#8296=DIRECTION('',(0.,0.,1.));
#8297=DIRECTION('center_axis',(0.,0.,1.));
#8298=DIRECTION('ref_axis',(1.,0.,0.));
#8299=DIRECTION('center_axis',(0.,0.,-1.));
#8300=DIRECTION('ref_axis',(-1.,0.,0.));
#8301=DIRECTION('center_axis',(0.,0.,-1.));
#8302=DIRECTION('ref_axis',(1.,0.,0.));
#8303=DIRECTION('center_axis',(0.,0.,1.));
#8304=DIRECTION('ref_axis',(1.,0.,0.));
#8305=DIRECTION('center_axis',(0.,0.,1.));
#8306=DIRECTION('ref_axis',(1.,0.,0.));
#8307=DIRECTION('center_axis',(0.,0.,1.));
#8308=DIRECTION('ref_axis',(1.,0.,0.));
#8309=DIRECTION('center_axis',(0.,0.,1.));
#8310=DIRECTION('ref_axis',(1.,0.,0.));
#8311=DIRECTION('',(0.,0.,-1.));
#8312=DIRECTION('center_axis',(0.,0.,1.));
#8313=DIRECTION('ref_axis',(1.,0.,0.));
#8314=DIRECTION('center_axis',(0.,0.,1.));
#8315=DIRECTION('ref_axis',(1.,0.,0.));
#8316=DIRECTION('center_axis',(0.,0.,1.));
#8317=DIRECTION('ref_axis',(1.,0.,0.));
#8318=DIRECTION('center_axis',(0.,0.,1.));
#8319=DIRECTION('ref_axis',(1.,0.,0.));
#8320=DIRECTION('',(0.,0.,-1.));
#8321=DIRECTION('center_axis',(0.,0.,1.));
#8322=DIRECTION('ref_axis',(1.,0.,0.));
#8323=DIRECTION('center_axis',(0.,0.,1.));
#8324=DIRECTION('ref_axis',(1.,0.,0.));
#8325=DIRECTION('center_axis',(0.,0.,1.));
#8326=DIRECTION('ref_axis',(1.,0.,0.));
#8327=DIRECTION('',(0.,0.,-1.));
#8328=DIRECTION('center_axis',(0.,0.,1.));
#8329=DIRECTION('ref_axis',(1.,0.,0.));
#8330=DIRECTION('axis',(0.,0.,1.));
#8331=DIRECTION('refdir',(1.,0.,0.));
#8332=DIRECTION('center_axis',(0.,0.,1.));
#8333=DIRECTION('ref_axis',(1.,0.,0.));
#8334=DIRECTION('center_axis',(0.,0.,-1.));
#8335=DIRECTION('ref_axis',(1.,0.,0.));
#8336=DIRECTION('',(0.,0.,-1.));
#8337=DIRECTION('center_axis',(0.,0.,-1.));
#8338=DIRECTION('ref_axis',(1.,0.,0.));
#8339=DIRECTION('center_axis',(0.,0.,1.));
#8340=DIRECTION('ref_axis',(1.,0.,0.));
#8341=DIRECTION('center_axis',(0.,0.,1.));
#8342=DIRECTION('ref_axis',(1.,0.,0.));
#8343=DIRECTION('',(0.,0.,-1.));
#8344=DIRECTION('center_axis',(0.,0.,1.));
#8345=DIRECTION('ref_axis',(1.,0.,0.));
#8346=DIRECTION('center_axis',(0.,0.,1.));
#8347=DIRECTION('ref_axis',(1.,0.,0.));
#8348=DIRECTION('center_axis',(0.,0.,1.));
#8349=DIRECTION('ref_axis',(1.,0.,0.));
#8350=DIRECTION('axis',(0.,0.,1.));
#8351=DIRECTION('refdir',(1.,0.,0.));
#8352=DIRECTION('center_axis',(0.,0.,1.));
#8353=DIRECTION('ref_axis',(1.,0.,0.));
#8354=DIRECTION('center_axis',(0.,0.,-1.));
#8355=DIRECTION('ref_axis',(1.,0.,0.));
#8356=DIRECTION('',(0.,0.,-1.));
#8357=DIRECTION('center_axis',(0.,0.,-1.));
#8358=DIRECTION('ref_axis',(1.,0.,0.));
#8359=DIRECTION('center_axis',(0.,0.,1.));
#8360=DIRECTION('ref_axis',(1.,0.,0.));
#8361=DIRECTION('center_axis',(0.,0.,1.));
#8362=DIRECTION('ref_axis',(1.,0.,0.));
#8363=DIRECTION('',(0.,0.,-1.));
#8364=DIRECTION('center_axis',(0.,0.,1.));
#8365=DIRECTION('ref_axis',(1.,0.,0.));
#8366=DIRECTION('center_axis',(0.,0.,1.));
#8367=DIRECTION('ref_axis',(1.,0.,0.));
#8368=DIRECTION('center_axis',(0.,0.,1.));
#8369=DIRECTION('ref_axis',(1.,0.,0.));
#8370=DIRECTION('axis',(0.,0.,1.));
#8371=DIRECTION('refdir',(1.,0.,0.));
#8372=DIRECTION('center_axis',(-1.,0.,0.));
#8373=DIRECTION('ref_axis',(0.,1.,0.));
#8374=DIRECTION('',(0.,0.,1.));
#8375=DIRECTION('',(0.,-1.,0.));
#8376=DIRECTION('',(0.,0.,-1.));
#8377=DIRECTION('',(0.,1.,0.));
#8378=DIRECTION('center_axis',(1.,0.,0.));
#8379=DIRECTION('ref_axis',(0.,-1.,0.));
#8380=DIRECTION('',(0.,0.,-1.));
#8381=DIRECTION('',(0.,-1.,0.));
#8382=DIRECTION('',(0.,0.,1.));
#8383=DIRECTION('',(0.,1.,0.));
#8384=DIRECTION('center_axis',(0.,0.,1.));
#8385=DIRECTION('ref_axis',(1.,0.,0.));
#8386=DIRECTION('center_axis',(0.,0.,1.));
#8387=DIRECTION('ref_axis',(1.,0.,0.));
#8388=DIRECTION('center_axis',(0.,0.,-1.));
#8389=DIRECTION('ref_axis',(1.,0.,0.));
#8390=DIRECTION('center_axis',(0.,0.,1.));
#8391=DIRECTION('ref_axis',(6.12323399573677E-17,-1.,0.));
#8392=DIRECTION('center_axis',(0.,0.,-1.));
#8393=DIRECTION('ref_axis',(1.,0.,0.));
#8394=DIRECTION('center_axis',(0.,0.,1.));
#8395=DIRECTION('ref_axis',(6.12323399573677E-17,-1.,0.));
#8396=DIRECTION('center_axis',(0.,0.,1.));
#8397=DIRECTION('ref_axis',(1.,0.,0.));
#8398=DIRECTION('center_axis',(0.,0.,1.));
#8399=DIRECTION('ref_axis',(1.,0.,0.));
#8400=DIRECTION('axis',(0.,0.,1.));
#8401=DIRECTION('refdir',(1.,0.,0.));
#8402=DIRECTION('center_axis',(0.,0.,1.));
#8403=DIRECTION('ref_axis',(1.,0.,0.));
#8404=DIRECTION('center_axis',(0.,0.,-1.));
#8405=DIRECTION('ref_axis',(1.,0.,0.));
#8406=DIRECTION('',(0.,0.,-1.));
#8407=DIRECTION('center_axis',(0.,0.,-1.));
#8408=DIRECTION('ref_axis',(1.,0.,0.));
#8409=DIRECTION('center_axis',(0.,0.,1.));
#8410=DIRECTION('ref_axis',(1.,0.,0.));
#8411=DIRECTION('center_axis',(0.,0.,-1.));
#8412=DIRECTION('ref_axis',(1.,0.,0.));
#8413=DIRECTION('',(0.,0.,-1.));
#8414=DIRECTION('center_axis',(0.,0.,-1.));
#8415=DIRECTION('ref_axis',(1.,0.,0.));
#8416=DIRECTION('center_axis',(0.,0.,1.));
#8417=DIRECTION('ref_axis',(1.,0.,0.));
#8418=DIRECTION('center_axis',(0.,0.,1.));
#8419=DIRECTION('ref_axis',(1.,0.,0.));
#8420=DIRECTION('axis',(0.,0.,1.));
#8421=DIRECTION('refdir',(1.,0.,0.));
#8422=DIRECTION('center_axis',(0.,0.,1.));
#8423=DIRECTION('ref_axis',(-0.45781772301594,-0.889046080072625,0.));
#8424=DIRECTION('',(0.,0.,1.));
#8425=DIRECTION('center_axis',(0.,0.,1.));
#8426=DIRECTION('ref_axis',(1.,2.67452657467291E-14,0.));
#8427=DIRECTION('center_axis',(0.,0.,1.));
#8428=DIRECTION('ref_axis',(1.,2.67452657467291E-14,0.));
#8429=DIRECTION('',(0.,0.,1.));
#8430=DIRECTION('center_axis',(0.,0.,1.));
#8431=DIRECTION('ref_axis',(1.,2.67452657467291E-14,0.));
#8432=DIRECTION('',(0.,0.,1.));
#8433=DIRECTION('center_axis',(0.,0.,1.));
#8434=DIRECTION('ref_axis',(1.,2.67452657467291E-14,0.));
#8435=DIRECTION('',(0.,0.,1.));
#8436=DIRECTION('center_axis',(0.,0.,1.));
#8437=DIRECTION('ref_axis',(1.,2.67452657467291E-14,0.));
#8438=DIRECTION('',(0.,0.,1.));
#8439=DIRECTION('center_axis',(0.,0.,1.));
#8440=DIRECTION('ref_axis',(1.,2.67452657467291E-14,0.));
#8441=DIRECTION('',(0.,0.,1.));
#8442=DIRECTION('center_axis',(0.,0.,1.));
#8443=DIRECTION('ref_axis',(1.,2.67452657467291E-14,0.));
#8444=DIRECTION('',(0.,0.,1.));
#8445=DIRECTION('center_axis',(0.,0.,1.));
#8446=DIRECTION('ref_axis',(1.,2.67452657467291E-14,0.));
#8447=DIRECTION('',(0.,0.,1.));
#8448=DIRECTION('center_axis',(0.,0.,1.));
#8449=DIRECTION('ref_axis',(-0.367640013946098,0.929968182329757,0.));
#8450=DIRECTION('',(0.,0.,-1.));
#8451=DIRECTION('center_axis',(0.,0.,1.));
#8452=DIRECTION('ref_axis',(1.,0.,0.));
#8453=DIRECTION('center_axis',(0.,0.,1.));
#8454=DIRECTION('ref_axis',(1.,0.,0.));
#8455=DIRECTION('',(0.,0.,-1.));
#8456=DIRECTION('center_axis',(0.,0.,1.));
#8457=DIRECTION('ref_axis',(1.,0.,0.));
#8458=DIRECTION('',(0.,0.,-1.));
#8459=DIRECTION('center_axis',(0.,0.,1.));
#8460=DIRECTION('ref_axis',(1.,0.,0.));
#8461=DIRECTION('',(0.,0.,-1.));
#8462=DIRECTION('center_axis',(0.,0.,1.));
#8463=DIRECTION('ref_axis',(1.,0.,0.));
#8464=DIRECTION('',(0.,0.,-1.));
#8465=DIRECTION('center_axis',(0.,0.,1.));
#8466=DIRECTION('ref_axis',(1.,0.,0.));
#8467=DIRECTION('',(0.,0.,-1.));
#8468=DIRECTION('center_axis',(0.,0.,1.));
#8469=DIRECTION('ref_axis',(1.,0.,0.));
#8470=DIRECTION('',(0.,0.,-1.));
#8471=DIRECTION('center_axis',(0.,0.,1.));
#8472=DIRECTION('ref_axis',(1.,0.,0.));
#8473=DIRECTION('center_axis',(0.,0.,-1.));
#8474=DIRECTION('ref_axis',(1.,0.,0.));
#8475=DIRECTION('',(-0.707106781186547,-8.65956056235493E-17,0.707106781186548));
#8476=DIRECTION('center_axis',(0.,0.,1.));
#8477=DIRECTION('ref_axis',(1.,2.67452657467291E-14,0.));
#8478=DIRECTION('center_axis',(0.,0.,1.));
#8479=DIRECTION('ref_axis',(1.,0.,0.));
#8480=DIRECTION('center_axis',(0.,0.,-1.));
#8481=DIRECTION('ref_axis',(1.,0.,0.));
#8482=DIRECTION('center_axis',(0.866025403784439,0.5,0.));
#8483=DIRECTION('ref_axis',(0.5,-0.866025403784439,0.));
#8484=DIRECTION('',(0.5,-0.866025403784439,0.));
#8485=DIRECTION('',(0.,0.,-1.));
#8486=DIRECTION('',(0.5,-0.866025403784439,0.));
#8487=DIRECTION('',(0.,0.,-1.));
#8488=DIRECTION('center_axis',(1.20185167898973E-16,1.,0.));
#8489=DIRECTION('ref_axis',(1.,-1.20185167898973E-16,0.));
#8490=DIRECTION('',(1.,-1.20185167898973E-16,0.));
#8491=DIRECTION('',(0.,0.,-1.));
#8492=DIRECTION('',(1.,-1.20185167898973E-16,0.));
#8493=DIRECTION('center_axis',(-0.866025403784439,0.5,0.));
#8494=DIRECTION('ref_axis',(0.5,0.866025403784439,0.));
#8495=DIRECTION('',(0.5,0.866025403784439,0.));
#8496=DIRECTION('',(0.,0.,-1.));
#8497=DIRECTION('',(0.5,0.866025403784439,0.));
#8498=DIRECTION('center_axis',(-0.866025403784439,-0.5,0.));
#8499=DIRECTION('ref_axis',(-0.5,0.866025403784439,0.));
#8500=DIRECTION('',(-0.5,0.866025403784439,0.));
#8501=DIRECTION('',(0.,0.,-1.));
#8502=DIRECTION('',(-0.5,0.866025403784439,0.));
#8503=DIRECTION('center_axis',(-2.40370335797945E-16,-1.,0.));
#8504=DIRECTION('ref_axis',(-1.,2.40370335797945E-16,0.));
#8505=DIRECTION('',(-1.,2.40370335797945E-16,0.));
#8506=DIRECTION('',(0.,0.,-1.));
#8507=DIRECTION('',(-1.,2.40370335797945E-16,0.));
#8508=DIRECTION('center_axis',(0.866025403784439,-0.5,0.));
#8509=DIRECTION('ref_axis',(-0.5,-0.866025403784439,0.));
#8510=DIRECTION('',(-0.5,-0.866025403784439,0.));
#8511=DIRECTION('',(-0.5,-0.866025403784439,0.));
#8512=DIRECTION('center_axis',(0.,0.,-1.));
#8513=DIRECTION('ref_axis',(-1.,0.,0.));
#8514=DIRECTION('center_axis',(0.,0.,1.));
#8515=DIRECTION('ref_axis',(-0.0731438164595877,0.997321403617573,0.));
#8516=DIRECTION('center_axis',(0.,0.,1.));
#8517=DIRECTION('ref_axis',(1.,0.,0.));
#8518=DIRECTION('center_axis',(0.,0.,1.));
#8519=DIRECTION('ref_axis',(1.,0.,0.));
#8520=DIRECTION('center_axis',(0.,0.,1.));
#8521=DIRECTION('ref_axis',(1.,0.,0.));
#8522=DIRECTION('center_axis',(0.,0.,1.));
#8523=DIRECTION('ref_axis',(1.,0.,0.));
#8524=DIRECTION('center_axis',(0.,0.,1.));
#8525=DIRECTION('ref_axis',(1.,0.,0.));
#8526=DIRECTION('',(0.,0.,-1.));
#8527=DIRECTION('center_axis',(0.,0.,1.));
#8528=DIRECTION('ref_axis',(1.,0.,0.));
#8529=DIRECTION('center_axis',(0.,0.,1.));
#8530=DIRECTION('ref_axis',(1.,0.,0.));
#8531=DIRECTION('center_axis',(0.,0.,1.));
#8532=DIRECTION('ref_axis',(1.,0.,0.));
#8533=DIRECTION('center_axis',(0.,0.,1.));
#8534=DIRECTION('ref_axis',(1.,0.,0.));
#8535=DIRECTION('',(0.,0.,-1.));
#8536=DIRECTION('center_axis',(0.,0.,1.));
#8537=DIRECTION('ref_axis',(1.,0.,0.));
#8538=DIRECTION('axis',(0.,0.,1.));
#8539=DIRECTION('refdir',(1.,0.,0.));
#8540=DIRECTION('center_axis',(0.,0.,1.));
#8541=DIRECTION('ref_axis',(1.,0.,0.));
#8542=DIRECTION('',(0.,0.,-1.));
#8543=DIRECTION('center_axis',(0.,0.,-1.));
#8544=DIRECTION('ref_axis',(1.,0.,0.));
#8545=DIRECTION('center_axis',(0.,0.,1.));
#8546=DIRECTION('ref_axis',(1.,0.,0.));
#8547=DIRECTION('',(0.,0.,-1.));
#8548=DIRECTION('center_axis',(0.,0.,1.));
#8549=DIRECTION('ref_axis',(1.,0.,0.));
#8550=DIRECTION('',(0.,0.,-1.));
#8551=DIRECTION('center_axis',(0.,0.,1.));
#8552=DIRECTION('ref_axis',(1.,0.,0.));
#8553=DIRECTION('',(0.,0.,-1.));
#8554=DIRECTION('center_axis',(0.,0.,1.));
#8555=DIRECTION('ref_axis',(1.,0.,0.));
#8556=DIRECTION('',(0.,0.,-1.));
#8557=DIRECTION('center_axis',(0.,0.,1.));
#8558=DIRECTION('ref_axis',(1.,0.,0.));
#8559=DIRECTION('',(0.,0.,-1.));
#8560=DIRECTION('center_axis',(0.,0.,1.));
#8561=DIRECTION('ref_axis',(1.,0.,0.));
#8562=DIRECTION('',(0.,0.,-1.));
#8563=DIRECTION('center_axis',(0.,0.,1.));
#8564=DIRECTION('ref_axis',(1.,0.,0.));
#8565=DIRECTION('',(0.,0.,-1.));
#8566=DIRECTION('center_axis',(0.,0.,1.));
#8567=DIRECTION('ref_axis',(1.,0.,0.));
#8568=DIRECTION('',(0.,0.,-1.));
#8569=DIRECTION('center_axis',(0.,0.,1.));
#8570=DIRECTION('ref_axis',(1.,0.,0.));
#8571=DIRECTION('',(0.,0.,-1.));
#8572=DIRECTION('center_axis',(0.,0.,1.));
#8573=DIRECTION('ref_axis',(1.,0.,0.));
#8574=DIRECTION('',(0.,0.,-1.));
#8575=DIRECTION('center_axis',(0.,0.,1.));
#8576=DIRECTION('ref_axis',(1.,0.,0.));
#8577=DIRECTION('',(0.,0.,-1.));
#8578=DIRECTION('center_axis',(0.,0.,1.));
#8579=DIRECTION('ref_axis',(1.,0.,0.));
#8580=DIRECTION('',(0.,0.,-1.));
#8581=DIRECTION('center_axis',(0.,0.,1.));
#8582=DIRECTION('ref_axis',(1.,9.40280585438808E-14,0.));
#8583=DIRECTION('',(0.,0.,1.));
#8584=DIRECTION('center_axis',(0.,0.,-1.));
#8585=DIRECTION('ref_axis',(1.,9.40280585438808E-14,0.));
#8586=DIRECTION('center_axis',(0.,0.,1.));
#8587=DIRECTION('ref_axis',(1.,9.40280585438808E-14,0.));
#8588=DIRECTION('',(0.,0.,1.));
#8589=DIRECTION('center_axis',(0.,0.,1.));
#8590=DIRECTION('ref_axis',(1.,9.40280585438808E-14,0.));
#8591=DIRECTION('',(0.,0.,1.));
#8592=DIRECTION('center_axis',(0.,0.,1.));
#8593=DIRECTION('ref_axis',(1.,9.40280585438808E-14,0.));
#8594=DIRECTION('',(0.,0.,1.));
#8595=DIRECTION('center_axis',(0.,0.,1.));
#8596=DIRECTION('ref_axis',(1.,9.40280585438808E-14,0.));
#8597=DIRECTION('',(0.,0.,1.));
#8598=DIRECTION('center_axis',(0.,0.,1.));
#8599=DIRECTION('ref_axis',(1.,9.40280585438808E-14,0.));
#8600=DIRECTION('',(0.,0.,1.));
#8601=DIRECTION('center_axis',(0.,0.,1.));
#8602=DIRECTION('ref_axis',(1.,9.40280585438808E-14,0.));
#8603=DIRECTION('',(0.,0.,1.));
#8604=DIRECTION('center_axis',(0.,0.,1.));
#8605=DIRECTION('ref_axis',(1.,9.40280585438808E-14,0.));
#8606=DIRECTION('',(0.,0.,1.));
#8607=DIRECTION('center_axis',(0.,0.,1.));
#8608=DIRECTION('ref_axis',(1.,9.40280585438808E-14,0.));
#8609=DIRECTION('',(0.,0.,1.));
#8610=DIRECTION('center_axis',(0.,0.,1.));
#8611=DIRECTION('ref_axis',(1.,9.40280585438808E-14,0.));
#8612=DIRECTION('',(0.,0.,1.));
#8613=DIRECTION('center_axis',(0.,0.,1.));
#8614=DIRECTION('ref_axis',(1.,9.40280585438808E-14,0.));
#8615=DIRECTION('',(0.,0.,1.));
#8616=DIRECTION('center_axis',(0.,0.,1.));
#8617=DIRECTION('ref_axis',(1.,9.40280585438808E-14,0.));
#8618=DIRECTION('',(0.,0.,1.));
#8619=DIRECTION('center_axis',(0.,0.,1.));
#8620=DIRECTION('ref_axis',(1.,9.40280585438808E-14,0.));
#8621=DIRECTION('',(0.,0.,1.));
#8622=DIRECTION('center_axis',(0.,0.,-1.));
#8623=DIRECTION('ref_axis',(1.,0.,0.));
#8624=DIRECTION('center_axis',(0.,0.,-1.));
#8625=DIRECTION('ref_axis',(1.,0.,0.));
#8626=DIRECTION('',(0.707106781186548,8.65956056235494E-17,0.707106781186547));
#8627=DIRECTION('center_axis',(0.,0.,1.));
#8628=DIRECTION('ref_axis',(1.,0.,0.));
#8629=DIRECTION('center_axis',(0.,0.,1.));
#8630=DIRECTION('ref_axis',(1.,9.40280585438808E-14,0.));
#8631=DIRECTION('center_axis',(0.,0.,-1.));
#8632=DIRECTION('ref_axis',(1.,9.40280585438808E-14,0.));
#8633=DIRECTION('center_axis',(0.,0.,1.));
#8634=DIRECTION('ref_axis',(1.,0.,0.));
#8635=DIRECTION('center_axis',(-1.60246890531964E-16,-1.,0.));
#8636=DIRECTION('ref_axis',(1.,-1.60246890531964E-16,0.));
#8637=DIRECTION('',(1.,-1.60246890531964E-16,0.));
#8638=DIRECTION('',(0.,0.,1.));
#8639=DIRECTION('',(1.,-1.60246890531964E-16,0.));
#8640=DIRECTION('',(0.,0.,1.));
#8641=DIRECTION('center_axis',(-0.866025403784439,-0.5,0.));
#8642=DIRECTION('ref_axis',(0.5,-0.866025403784439,0.));
#8643=DIRECTION('',(0.5,-0.866025403784439,0.));
#8644=DIRECTION('',(0.,0.,1.));
#8645=DIRECTION('',(0.5,-0.866025403784439,0.));
#8646=DIRECTION('center_axis',(-0.866025403784439,0.5,0.));
#8647=DIRECTION('ref_axis',(-0.5,-0.866025403784439,0.));
#8648=DIRECTION('',(-0.5,-0.866025403784439,0.));
#8649=DIRECTION('',(0.,0.,1.));
#8650=DIRECTION('',(-0.5,-0.866025403784439,0.));
#8651=DIRECTION('center_axis',(1.60246890531964E-16,1.,0.));
#8652=DIRECTION('ref_axis',(-1.,1.60246890531964E-16,0.));
#8653=DIRECTION('',(-1.,1.60246890531964E-16,0.));
#8654=DIRECTION('',(0.,0.,1.));
#8655=DIRECTION('',(-1.,1.60246890531964E-16,0.));
#8656=DIRECTION('center_axis',(0.866025403784439,0.5,0.));
#8657=DIRECTION('ref_axis',(-0.5,0.866025403784439,0.));
#8658=DIRECTION('',(-0.5,0.866025403784439,0.));
#8659=DIRECTION('',(0.,0.,1.));
#8660=DIRECTION('',(-0.5,0.866025403784439,0.));
#8661=DIRECTION('center_axis',(0.866025403784439,-0.5,0.));
#8662=DIRECTION('ref_axis',(0.5,0.866025403784439,0.));
#8663=DIRECTION('',(0.5,0.866025403784439,0.));
#8664=DIRECTION('',(0.5,0.866025403784439,0.));
#8665=DIRECTION('center_axis',(0.,0.,1.));
#8666=DIRECTION('ref_axis',(1.,0.,0.));
#8667=DIRECTION('center_axis',(0.,0.,1.));
#8668=DIRECTION('ref_axis',(1.,0.,0.));
#8669=DIRECTION('center_axis',(0.,0.,1.));
#8670=DIRECTION('ref_axis',(1.,0.,0.));
#8671=DIRECTION('center_axis',(0.,0.,1.));
#8672=DIRECTION('ref_axis',(1.,0.,0.));
#8673=DIRECTION('',(0.,0.,-1.));
#8674=DIRECTION('center_axis',(0.,0.,1.));
#8675=DIRECTION('ref_axis',(1.,0.,0.));
#8676=DIRECTION('center_axis',(0.,0.,1.));
#8677=DIRECTION('ref_axis',(1.,0.,0.));
#8678=DIRECTION('center_axis',(0.,0.,1.));
#8679=DIRECTION('ref_axis',(1.,0.,0.));
#8680=DIRECTION('',(0.,0.,1.));
#8681=DIRECTION('',(1.,0.,0.));
#8682=DIRECTION('',(0.,0.,1.));
#8683=DIRECTION('',(1.,0.,0.));
#8684=DIRECTION('',(6.12323399573676E-17,-4.92927014030986E-32,1.));
#8685=DIRECTION('',(1.,3.74939945665459E-33,-6.12323399573676E-17));
#8686=DIRECTION('',(-3.85587357684361E-17,1.,2.20876025266356E-16));
#8687=DIRECTION('',(0.99473718508465,6.09866375718863E-17,-0.102459419332082));
#8688=DIRECTION('',(-3.85587357684361E-17,1.,2.20876025266356E-16));
#8689=DIRECTION('',(0.99473718508465,6.09866375718863E-17,-0.102459419332082));
#8690=DIRECTION('',(-3.85587357684361E-17,1.,2.20876025266356E-16));
#8691=DIRECTION('',(0.99473718508465,6.09866375718863E-17,-0.102459419332082));
#8692=DIRECTION('',(6.12323399573676E-17,-4.92927014030986E-32,1.));
#8693=DIRECTION('',(1.,3.74939945665459E-33,-6.12323399573676E-17));
#8694=DIRECTION('',(-3.85587357684361E-17,1.,2.20876025266356E-16));
#8695=DIRECTION('',(0.99473718508465,6.09866375718863E-17,-0.102459419332082));
#8696=DIRECTION('',(-3.85587357684361E-17,1.,2.20876025266356E-16));
#8697=DIRECTION('',(0.99473718508465,6.09866375718863E-17,-0.102459419332082));
#8698=DIRECTION('',(0.,1.,2.22044604925031E-16));
#8699=DIRECTION('',(1.,0.,0.));
#8700=DIRECTION('',(0.,1.,2.22044604925031E-16));
#8701=DIRECTION('',(1.,0.,0.));
#8702=DIRECTION('',(-3.85587357684361E-17,1.,2.20876025266356E-16));
#8703=DIRECTION('',(0.99473718508465,6.09866375718863E-17,-0.102459419332082));
#8704=DIRECTION('',(-3.85587357684361E-17,1.,2.20876025266356E-16));
#8705=DIRECTION('',(0.99473718508465,6.09866375718863E-17,-0.102459419332082));
#8706=DIRECTION('',(-3.85587357684361E-17,1.,2.20876025266356E-16));
#8707=DIRECTION('',(0.99473718508465,6.09866375718863E-17,-0.102459419332082));
#8708=DIRECTION('',(0.,1.,2.22044604925031E-16));
#8709=DIRECTION('',(1.,0.,0.));
#8710=DIRECTION('',(0.,1.,2.22044604925031E-16));
#8711=DIRECTION('',(1.,0.,0.));
#8712=DIRECTION('',(0.,1.,2.22044604925031E-16));
#8713=DIRECTION('',(1.,0.,0.));
#8714=DIRECTION('',(0.,1.,2.22044604925031E-16));
#8715=DIRECTION('',(1.,0.,0.));
#8716=DIRECTION('',(0.,1.,2.22044604925031E-16));
#8717=DIRECTION('',(1.,0.,0.));
#8718=DIRECTION('',(0.,1.,2.22044604925031E-16));
#8719=DIRECTION('',(1.,0.,0.));
#8720=DIRECTION('',(0.,1.,2.22044604925031E-16));
#8721=DIRECTION('',(1.,0.,0.));
#8722=DIRECTION('',(0.,1.,2.22044604925031E-16));
#8723=DIRECTION('',(1.,0.,0.));
#8724=DIRECTION('',(-1.22464679914735E-16,1.,2.22044604925029E-16));
#8725=DIRECTION('',(1.,1.22464679914735E-16,6.16297582204079E-33));
#8726=DIRECTION('',(-3.85587357684361E-17,1.,2.20876025266356E-16));
#8727=DIRECTION('',(-0.997416783532731,-2.25932808631228E-17,-0.0718314689201175));
#8728=DIRECTION('',(0.,-1.22464679914735E-16,-1.));
#8729=DIRECTION('',(0.766044443118978,-0.642787609686539,7.87187788734199E-17));
#8730=DIRECTION('',(0.,-1.22464679914735E-16,-1.));
#8731=DIRECTION('',(0.766044443118978,-0.642787609686539,7.87187788734199E-17));
#8732=CARTESIAN_POINT('',(0.,0.,0.));
#8733=CARTESIAN_POINT('',(0.,0.,0.));
#8734=CARTESIAN_POINT('Origin',(83.,-23.,-4.));
#8735=CARTESIAN_POINT('',(79.5,-23.,-4.));
#8736=CARTESIAN_POINT('Origin',(83.,-23.,-4.));
#8737=CARTESIAN_POINT('',(80.5,-23.,-4.));
#8738=CARTESIAN_POINT('Origin',(83.,-23.,-4.));
#8739=CARTESIAN_POINT('Origin',(83.,-23.,-2.));
#8740=CARTESIAN_POINT('',(79.5,-23.,0.));
#8741=CARTESIAN_POINT('Origin',(83.,-23.,0.));
#8742=CARTESIAN_POINT('',(79.5,-23.,-2.));
#8743=CARTESIAN_POINT('Origin',(83.,-23.,-3.));
#8744=CARTESIAN_POINT('',(80.5,-23.,-6.));
#8745=CARTESIAN_POINT('',(80.5,-23.,-3.));
#8746=CARTESIAN_POINT('Origin',(83.,-23.,-6.));
#8747=CARTESIAN_POINT('Origin',(83.,23.,-4.));
#8748=CARTESIAN_POINT('',(79.5,23.,-4.));
#8749=CARTESIAN_POINT('Origin',(83.,23.,-4.));
#8750=CARTESIAN_POINT('',(80.5,23.,-4.));
#8751=CARTESIAN_POINT('Origin',(83.,23.,-4.));
#8752=CARTESIAN_POINT('Origin',(83.,23.,-2.));
#8753=CARTESIAN_POINT('',(79.5,23.,0.));
#8754=CARTESIAN_POINT('Origin',(83.,23.,0.));
#8755=CARTESIAN_POINT('',(79.5,23.,-2.));
#8756=CARTESIAN_POINT('Origin',(83.,23.,-3.));
#8757=CARTESIAN_POINT('',(80.5,23.,-6.));
#8758=CARTESIAN_POINT('',(80.5,23.,-3.));
#8759=CARTESIAN_POINT('Origin',(83.,23.,-6.));
#8760=CARTESIAN_POINT('Origin',(105.,-23.,-3.));
#8761=CARTESIAN_POINT('',(101.5,-23.,0.));
#8762=CARTESIAN_POINT('Origin',(105.,-23.,0.));
#8763=CARTESIAN_POINT('',(101.5,-23.,-6.));
#8764=CARTESIAN_POINT('',(101.5,-23.,-3.));
#8765=CARTESIAN_POINT('Origin',(105.,-23.,-6.));
#8766=CARTESIAN_POINT('Origin',(-105.,-23.,-3.));
#8767=CARTESIAN_POINT('',(-108.5,-23.,0.));
#8768=CARTESIAN_POINT('Origin',(-105.,-23.,0.));
#8769=CARTESIAN_POINT('',(-108.5,-23.,-6.));
#8770=CARTESIAN_POINT('',(-108.5,-23.,-3.));
#8771=CARTESIAN_POINT('Origin',(-105.,-23.,-6.));
#8772=CARTESIAN_POINT('Origin',(-105.,23.,-3.));
#8773=CARTESIAN_POINT('',(-108.5,23.,0.));
#8774=CARTESIAN_POINT('Origin',(-105.,23.,0.));
#8775=CARTESIAN_POINT('',(-108.5,23.,-6.));
#8776=CARTESIAN_POINT('',(-108.5,23.,-3.));
#8777=CARTESIAN_POINT('Origin',(-105.,23.,-6.));
#8778=CARTESIAN_POINT('Origin',(105.,23.,-3.));
#8779=CARTESIAN_POINT('',(101.5,23.,0.));
#8780=CARTESIAN_POINT('Origin',(105.,23.,0.));
#8781=CARTESIAN_POINT('',(101.5,23.,-6.));
#8782=CARTESIAN_POINT('',(101.5,23.,-3.));
#8783=CARTESIAN_POINT('Origin',(105.,23.,-6.));
#8784=CARTESIAN_POINT('Origin',(72.,-6.,0.));
#8785=CARTESIAN_POINT('',(72.,-6.,0.));
#8786=CARTESIAN_POINT('',(64.,-6.,0.));
#8787=CARTESIAN_POINT('',(36.,-6.,0.));
#8788=CARTESIAN_POINT('',(72.,-6.,-6.));
#8789=CARTESIAN_POINT('',(72.,-6.,0.));
#8790=CARTESIAN_POINT('',(64.,-6.,-6.));
#8791=CARTESIAN_POINT('',(36.,-6.,-6.));
#8792=CARTESIAN_POINT('',(64.,-6.,0.));
#8793=CARTESIAN_POINT('Origin',(72.,6.,0.));
#8794=CARTESIAN_POINT('',(72.,6.,0.));
#8795=CARTESIAN_POINT('',(72.,3.,0.));
#8796=CARTESIAN_POINT('',(72.,6.,-6.));
#8797=CARTESIAN_POINT('',(72.,6.,0.));
#8798=CARTESIAN_POINT('',(72.,3.,-6.));
#8799=CARTESIAN_POINT('Origin',(64.,6.,0.));
#8800=CARTESIAN_POINT('',(64.,6.,0.));
#8801=CARTESIAN_POINT('',(32.,6.,0.));
#8802=CARTESIAN_POINT('',(64.,6.,-6.));
#8803=CARTESIAN_POINT('',(64.,6.,0.));
#8804=CARTESIAN_POINT('',(32.,6.,-6.));
#8805=CARTESIAN_POINT('Origin',(64.,-6.,0.));
#8806=CARTESIAN_POINT('',(64.,-3.,0.));
#8807=CARTESIAN_POINT('',(64.,-3.,-6.));
#8808=CARTESIAN_POINT('Origin',(102.,-6.,0.));
#8809=CARTESIAN_POINT('',(102.,-6.,0.));
#8810=CARTESIAN_POINT('',(94.,-6.,0.));
#8811=CARTESIAN_POINT('',(51.,-6.,0.));
#8812=CARTESIAN_POINT('',(102.,-6.,-6.));
#8813=CARTESIAN_POINT('',(102.,-6.,0.));
#8814=CARTESIAN_POINT('',(94.,-6.,-6.));
#8815=CARTESIAN_POINT('',(51.,-6.,-6.));
#8816=CARTESIAN_POINT('',(94.,-6.,0.));
#8817=CARTESIAN_POINT('Origin',(102.,6.,0.));
#8818=CARTESIAN_POINT('',(102.,6.,0.));
#8819=CARTESIAN_POINT('',(102.,3.,0.));
#8820=CARTESIAN_POINT('',(102.,6.,-6.));
#8821=CARTESIAN_POINT('',(102.,6.,0.));
#8822=CARTESIAN_POINT('',(102.,3.,-6.));
#8823=CARTESIAN_POINT('Origin',(94.,6.,0.));
#8824=CARTESIAN_POINT('',(94.,6.,0.));
#8825=CARTESIAN_POINT('',(47.,6.,0.));
#8826=CARTESIAN_POINT('',(94.,6.,-6.));
#8827=CARTESIAN_POINT('',(94.,6.,0.));
#8828=CARTESIAN_POINT('',(47.,6.,-6.));
#8829=CARTESIAN_POINT('Origin',(94.,-6.,0.));
#8830=CARTESIAN_POINT('',(94.,-3.,0.));
#8831=CARTESIAN_POINT('',(94.,-3.,-6.));
#8832=CARTESIAN_POINT('Origin',(120.,15.,0.));
#8833=CARTESIAN_POINT('',(-125.,15.,0.));
#8834=CARTESIAN_POINT('',(120.,15.,0.));
#8835=CARTESIAN_POINT('',(60.,15.,0.));
#8836=CARTESIAN_POINT('',(-125.,15.,25.));
#8837=CARTESIAN_POINT('',(-125.,15.,-3.));
#8838=CARTESIAN_POINT('',(120.,15.,25.));
#8839=CARTESIAN_POINT('',(120.,15.,25.));
#8840=CARTESIAN_POINT('',(120.,15.,0.));
#8841=CARTESIAN_POINT('Origin',(-120.,11.,0.));
#8842=CARTESIAN_POINT('',(120.,11.,0.));
#8843=CARTESIAN_POINT('',(-125.,11.,0.));
#8844=CARTESIAN_POINT('',(-60.,11.,0.));
#8845=CARTESIAN_POINT('',(120.,11.,25.));
#8846=CARTESIAN_POINT('',(120.,11.,0.));
#8847=CARTESIAN_POINT('',(-125.,11.,25.));
#8848=CARTESIAN_POINT('',(-120.,11.,25.));
#8849=CARTESIAN_POINT('',(-125.,11.,-3.));
#8850=CARTESIAN_POINT('Origin',(0.,13.,25.));
#8851=CARTESIAN_POINT('',(-125.,21.5,25.));
#8852=CARTESIAN_POINT('',(120.,11.,25.));
#8853=CARTESIAN_POINT('Origin',(0.,0.,0.));
#8854=CARTESIAN_POINT('',(120.,35.,0.));
#8855=CARTESIAN_POINT('',(120.,-30.,0.));
#8856=CARTESIAN_POINT('',(-125.,35.,0.));
#8857=CARTESIAN_POINT('',(60.,35.,0.));
#8858=CARTESIAN_POINT('',(-125.,15.,0.));
#8859=CARTESIAN_POINT('Origin',(0.,0.,0.));
#8860=CARTESIAN_POINT('',(-125.,-11.,0.));
#8861=CARTESIAN_POINT('',(-125.,15.,0.));
#8862=CARTESIAN_POINT('',(120.,-11.,0.));
#8863=CARTESIAN_POINT('',(60.,-11.,0.));
#8864=CARTESIAN_POINT('',(120.,-30.,0.));
#8865=CARTESIAN_POINT('Origin',(120.,-11.,0.));
#8866=CARTESIAN_POINT('',(-125.,-11.,22.));
#8867=CARTESIAN_POINT('',(-125.,-11.,-3.));
#8868=CARTESIAN_POINT('',(120.,-11.,22.));
#8869=CARTESIAN_POINT('',(120.,-11.,22.));
#8870=CARTESIAN_POINT('',(120.,-11.,0.));
#8871=CARTESIAN_POINT('Origin',(-120.,-15.,0.));
#8872=CARTESIAN_POINT('',(120.,-15.,0.));
#8873=CARTESIAN_POINT('',(-125.,-15.,0.));
#8874=CARTESIAN_POINT('',(-60.,-15.,0.));
#8875=CARTESIAN_POINT('',(120.,-15.,22.));
#8876=CARTESIAN_POINT('',(120.,-15.,0.));
#8877=CARTESIAN_POINT('',(-125.,-15.,22.));
#8878=CARTESIAN_POINT('',(-120.,-15.,22.));
#8879=CARTESIAN_POINT('',(-125.,-15.,-3.));
#8880=CARTESIAN_POINT('Origin',(0.,-13.,22.));
#8881=CARTESIAN_POINT('',(-125.,8.5,22.));
#8882=CARTESIAN_POINT('',(120.,-15.,22.));
#8883=CARTESIAN_POINT('Origin',(0.,0.,0.));
#8884=CARTESIAN_POINT('',(-125.,-35.,0.));
#8885=CARTESIAN_POINT('',(-125.,15.,0.));
#8886=CARTESIAN_POINT('',(120.,-35.,0.));
#8887=CARTESIAN_POINT('',(-60.,-35.,0.));
#8888=CARTESIAN_POINT('',(120.,-30.,0.));
#8889=CARTESIAN_POINT('Origin',(120.,35.,-6.));
#8890=CARTESIAN_POINT('',(120.,35.,-6.));
#8891=CARTESIAN_POINT('',(-125.,35.,-6.));
#8892=CARTESIAN_POINT('',(60.,35.,-6.));
#8893=CARTESIAN_POINT('',(-125.,35.,-6.));
#8894=CARTESIAN_POINT('',(120.,35.,-6.));
#8895=CARTESIAN_POINT('Origin',(120.,-30.,-6.));
#8896=CARTESIAN_POINT('',(120.,-35.,-6.));
#8897=CARTESIAN_POINT('',(120.,-30.,-6.));
#8898=CARTESIAN_POINT('',(120.,-35.,-6.));
#8899=CARTESIAN_POINT('Origin',(-120.,-35.,-6.));
#8900=CARTESIAN_POINT('',(-125.,-35.,-6.));
#8901=CARTESIAN_POINT('',(-60.,-35.,-6.));
#8902=CARTESIAN_POINT('',(-125.,-35.,-6.));
#8903=CARTESIAN_POINT('Origin',(-125.,30.,-6.));
#8904=CARTESIAN_POINT('',(-125.,15.,-6.));
#8905=CARTESIAN_POINT('Origin',(0.,0.,-6.));
#8906=CARTESIAN_POINT('',(0.,0.,0.));
#8907=CARTESIAN_POINT('Origin',(83.,23.,-12.));
#8908=CARTESIAN_POINT('',(81.3313534283113,22.999608308332,-16.2285196366098));
#8909=CARTESIAN_POINT('',(81.3334663741701,23.0014782390593,-16.4214803633902));
#8910=CARTESIAN_POINT('',(81.334,23.,-12.));
#8911=CARTESIAN_POINT('',(82.2300979593295,21.5225674811446,-17.));
#8912=CARTESIAN_POINT('Ctrl Pts',(81.3334663741701,23.0014782390593,-16.4214803633902));
#8913=CARTESIAN_POINT('Ctrl Pts',(81.3324167265455,23.1152856061038,-16.4290983789409));
#8914=CARTESIAN_POINT('Ctrl Pts',(81.3430834208759,23.2288980499925,-16.4367163944915));
#8915=CARTESIAN_POINT('Ctrl Pts',(81.366191211586,23.3399236516146,-16.4443344100422));
#8916=CARTESIAN_POINT('Ctrl Pts',(81.4785582190846,23.8798114654899,-16.4813787827061));
#8917=CARTESIAN_POINT('Ctrl Pts',(81.8851094874654,24.3585303713383,-16.5184231553699));
#8918=CARTESIAN_POINT('Ctrl Pts',(82.3995343180334,24.5569680544574,-16.5554675280338));
#8919=CARTESIAN_POINT('Ctrl Pts',(82.9139591486014,24.7554057375764,-16.5925119006976));
#8920=CARTESIAN_POINT('Ctrl Pts',(83.5362575413566,24.6735621979661,-16.6295562733615));
#8921=CARTESIAN_POINT('Ctrl Pts',(83.9821832750364,24.348973723947,-16.6666006460253));
#8922=CARTESIAN_POINT('Ctrl Pts',(84.4281090087162,24.0243852499279,-16.7036450186892));
#8923=CARTESIAN_POINT('Ctrl Pts',(84.6976620833208,23.4570518415,-16.740689391353));
#8924=CARTESIAN_POINT('Ctrl Pts',(84.6664136128519,22.9064184197971,-16.7777337640169));
#8925=CARTESIAN_POINT('Ctrl Pts',(84.635165142383,22.3557849980942,-16.8147781366807));
#8926=CARTESIAN_POINT('Ctrl Pts',(84.3031151268407,21.8218515631163,-16.8518225093446));
#8927=CARTESIAN_POINT('Ctrl Pts',(83.8246634223492,21.5495472460214,-16.8888668820084));
#8928=CARTESIAN_POINT('Ctrl Pts',(83.3462117178578,21.2772429289266,-16.9259112546723));
#8929=CARTESIAN_POINT('Ctrl Pts',(82.7213583244172,21.2665677297147,-16.9629556273362));
#8930=CARTESIAN_POINT('Ctrl Pts',(82.2300979593296,21.5225674811446,-17.));
#8931=CARTESIAN_POINT('',(81.6629741098033,23.9990032536159,-17.));
#8932=CARTESIAN_POINT('Origin',(83.,23.,-17.));
#8933=CARTESIAN_POINT('',(81.3354782356987,22.9987789599865,-16.9285196366098));
#8934=CARTESIAN_POINT('Ctrl Pts',(81.6629726863575,23.9990044309052,-17.));
#8935=CARTESIAN_POINT('Ctrl Pts',(81.4510076185789,23.7145503593587,-16.9761732122033));
#8936=CARTESIAN_POINT('Ctrl Pts',(81.3378311765629,23.3559374868803,-16.9523464244065));
#8937=CARTESIAN_POINT('Ctrl Pts',(81.3354782356987,22.9987789599865,-16.9285196366098));
#8938=CARTESIAN_POINT('',(81.334,23.,-18.));
#8939=CARTESIAN_POINT('',(81.334,23.,-12.));
#8940=CARTESIAN_POINT('Origin',(83.,23.,-18.));
#8941=CARTESIAN_POINT('Ctrl Pts',(81.3354782356987,22.9987789599865,-16.9285196366098));
#8942=CARTESIAN_POINT('Ctrl Pts',(81.3342446902247,22.8115361392917,-16.9160282787975));
#8943=CARTESIAN_POINT('Ctrl Pts',(81.3634704623982,22.6246930386351,-16.9035369209851));
#8944=CARTESIAN_POINT('Ctrl Pts',(81.4248896518804,22.4491447215318,-16.8910455631728));
#8945=CARTESIAN_POINT('Ctrl Pts',(81.6070344097262,21.9285386051282,-16.8540011905089));
#8946=CARTESIAN_POINT('Ctrl Pts',(82.0723133280082,21.5072676735534,-16.8169568178451));
#8947=CARTESIAN_POINT('Ctrl Pts',(82.6082885703566,21.3778807889459,-16.7799124451812));
#8948=CARTESIAN_POINT('Ctrl Pts',(83.144263812705,21.2484939043384,-16.7428680725174));
#8949=CARTESIAN_POINT('Ctrl Pts',(83.7509353791199,21.4109910666983,-16.7058236998535));
#8950=CARTESIAN_POINT('Ctrl Pts',(84.1504372220724,21.7911271928933,-16.6687793271897));
#8951=CARTESIAN_POINT('Ctrl Pts',(84.549939065025,22.1712633190883,-16.6317349545258));
#8952=CARTESIAN_POINT('Ctrl Pts',(84.7422711845153,22.7690384091184,-16.594690581862));
#8953=CARTESIAN_POINT('Ctrl Pts',(84.639539482518,23.3108402472818,-16.5576462091981));
#8954=CARTESIAN_POINT('Ctrl Pts',(84.5368077805207,23.8526420854451,-16.5206018365343));
#8955=CARTESIAN_POINT('Ctrl Pts',(84.1390122570358,24.3384706717417,-16.4835574638704));
#8956=CARTESIAN_POINT('Ctrl Pts',(83.6281313759476,24.5460306512639,-16.4465130912066));
#8957=CARTESIAN_POINT('Ctrl Pts',(83.1172504948595,24.7535906307861,-16.4094687185427));
#8958=CARTESIAN_POINT('Ctrl Pts',(82.493284256168,24.6828820035339,-16.3724243458788));
#8959=CARTESIAN_POINT('Ctrl Pts',(82.0418022728353,24.3662477041162,-16.335379973215));
#8960=CARTESIAN_POINT('Ctrl Pts',(81.607678605813,24.0617871758054,-16.2997598610132));
#8961=CARTESIAN_POINT('Ctrl Pts',(81.3330310126921,23.5299478610255,-16.2641397488115));
#8962=CARTESIAN_POINT('Ctrl Pts',(81.3313534283113,22.999608308332,-16.2285196366098));
#8963=CARTESIAN_POINT('Origin',(83.,23.,-12.));
#8964=CARTESIAN_POINT('',(81.3344264707835,23.0015125425552,-15.5285196366098));
#8965=CARTESIAN_POINT('',(81.3367022839223,22.9999597918218,-15.7214803633902));
#8966=CARTESIAN_POINT('',(81.334,23.,-12.));
#8967=CARTESIAN_POINT('Ctrl Pts',(81.3367022839223,22.9999597918218,-15.7214803633902));
#8968=CARTESIAN_POINT('Ctrl Pts',(81.3367622982155,23.2804572295637,-15.7401654762911));
#8969=CARTESIAN_POINT('Ctrl Pts',(81.4039329804852,23.5609817981292,-15.758850589192));
#8970=CARTESIAN_POINT('Ctrl Pts',(81.5380528850521,23.8046577193695,-15.7775357020929));
#8971=CARTESIAN_POINT('Ctrl Pts',(81.8039537523775,24.2877600524149,-15.8145800747567));
#8972=CARTESIAN_POINT('Ctrl Pts',(82.3330017103809,24.6260270310476,-15.8516244474206));
#8973=CARTESIAN_POINT('Ctrl Pts',(82.8830897957813,24.6646603768711,-15.8886688200844));
#8974=CARTESIAN_POINT('Ctrl Pts',(83.4331778811817,24.7032937226946,-15.9257131927483));
#8975=CARTESIAN_POINT('Ctrl Pts',(84.0043060939791,24.442293435709,-15.9627575654121));
#8976=CARTESIAN_POINT('Ctrl Pts',(84.33512331298,24.001099683907,-15.999801938076));
#8977=CARTESIAN_POINT('Ctrl Pts',(84.6659405319808,23.559905932105,-16.0368463107398));
#8978=CARTESIAN_POINT('Ctrl Pts',(84.7564467571851,22.9385187154866,-16.0738906834037));
#8979=CARTESIAN_POINT('Ctrl Pts',(84.5652078284987,22.4212944599841,-16.1109350560675));
#8980=CARTESIAN_POINT('Ctrl Pts',(84.3739688998123,21.9040702044815,-16.1479794287314));
#8981=CARTESIAN_POINT('Ctrl Pts',(83.9009848172353,21.4910089100948,-16.1850238013952));
#8982=CARTESIAN_POINT('Ctrl Pts',(83.3627357719796,21.3711407259392,-16.2220681740591));
#8983=CARTESIAN_POINT('Ctrl Pts',(82.8244867267238,21.2512725417836,-16.2591125467229));
#8984=CARTESIAN_POINT('Ctrl Pts',(82.2209727187894,21.4245974678592,-16.2961569193868));
#8985=CARTESIAN_POINT('Ctrl Pts',(81.8283070881303,21.8117882918482,-16.3332012920507));
#8986=CARTESIAN_POINT('Ctrl Pts',(81.5163914517474,22.1193549919522,-16.3626276491638));
#8987=CARTESIAN_POINT('Ctrl Pts',(81.3375208822818,22.5618708107873,-16.392054006277));
#8988=CARTESIAN_POINT('Ctrl Pts',(81.3334663741701,23.0014782390593,-16.4214803633902));
#8989=CARTESIAN_POINT('Ctrl Pts',(81.3313534283113,22.999608308332,-16.2285196366098));
#8990=CARTESIAN_POINT('Ctrl Pts',(81.3312863505578,22.9784028260999,-16.2270953761477));
#8991=CARTESIAN_POINT('Ctrl Pts',(81.3316556913563,22.957199741655,-16.2256711156856));
#8992=CARTESIAN_POINT('Ctrl Pts',(81.3324687060016,22.9360136864517,-16.2242468552234));
#8993=CARTESIAN_POINT('Ctrl Pts',(81.3536148504745,22.3849739397882,-16.1872024825596));
#8994=CARTESIAN_POINT('Ctrl Pts',(81.6749048673942,21.8454544180445,-16.1501581098957));
#8995=CARTESIAN_POINT('Ctrl Pts',(82.1493177603708,21.564346170154,-16.1131137372319));
#8996=CARTESIAN_POINT('Ctrl Pts',(82.6237306533474,21.2832379222636,-16.076069364568));
#8997=CARTESIAN_POINT('Ctrl Pts',(83.2512664223808,21.2605409482263,-16.0390249919042));
#8998=CARTESIAN_POINT('Ctrl Pts',(83.744748519932,21.5066436861515,-16.0019806192403));
#8999=CARTESIAN_POINT('Ctrl Pts',(84.2382306174832,21.7527464240767,-15.9649362465765));
#9000=CARTESIAN_POINT('Ctrl Pts',(84.5976590435522,22.2676488739642,-15.9278918739126));
#9001=CARTESIAN_POINT('Ctrl Pts',(84.6585541971785,22.8157206109035,-15.8908475012488));
#9002=CARTESIAN_POINT('Ctrl Pts',(84.7194493508049,23.3637923478428,-15.8538031285849));
#9003=CARTESIAN_POINT('Ctrl Pts',(84.4818112319886,23.945033371834,-15.816758755921));
#9004=CARTESIAN_POINT('Ctrl Pts',(84.0543867577353,24.2934568182214,-15.7797143832572));
#9005=CARTESIAN_POINT('Ctrl Pts',(83.626962283482,24.6418802646089,-15.7426700105933));
#9006=CARTESIAN_POINT('Ctrl Pts',(83.0097514537917,24.7574861333928,-15.7056256379295));
#9007=CARTESIAN_POINT('Ctrl Pts',(82.4852025736897,24.5873706699448,-15.6685812652656));
#9008=CARTESIAN_POINT('Ctrl Pts',(81.9606536935877,24.4172552064967,-15.6315368926018));
#9009=CARTESIAN_POINT('Ctrl Pts',(81.528766763074,23.9614184108167,-15.5944925199379));
#9010=CARTESIAN_POINT('Ctrl Pts',(81.3871814989429,23.4284602887024,-15.5574481472741));
#9011=CARTESIAN_POINT('Ctrl Pts',(81.350326141176,23.289728603694,-15.547805310386));
#9012=CARTESIAN_POINT('Ctrl Pts',(81.3331412508702,23.1457712768177,-15.5381624734979));
#9013=CARTESIAN_POINT('Ctrl Pts',(81.3344264707835,23.0015125425552,-15.5285196366098));
#9014=CARTESIAN_POINT('Origin',(83.,23.,-12.));
#9015=CARTESIAN_POINT('',(81.3365468042549,22.999471848124,-14.8285196366098));
#9016=CARTESIAN_POINT('',(81.333366306688,22.9985354187012,-15.0214803633902));
#9017=CARTESIAN_POINT('',(81.334,23.,-12.));
#9018=CARTESIAN_POINT('Ctrl Pts',(81.333366306688,22.9985354187012,-15.0214803633902));
#9019=CARTESIAN_POINT('Ctrl Pts',(81.3374449915474,23.4429099901808,-15.0512325736413));
#9020=CARTESIAN_POINT('Ctrl Pts',(81.5206881913661,23.8902541505524,-15.0809847838924));
#9021=CARTESIAN_POINT('Ctrl Pts',(81.8387594834446,24.1984499635096,-15.1107369941435));
#9022=CARTESIAN_POINT('Ctrl Pts',(82.2347889339624,24.5821834895996,-15.1477813668074));
#9023=CARTESIAN_POINT('Ctrl Pts',(82.8398376944982,24.7502001641106,-15.1848257394712));
#9024=CARTESIAN_POINT('Ctrl Pts',(83.3770234781491,24.6256122398906,-15.2218701121351));
#9025=CARTESIAN_POINT('Ctrl Pts',(83.9142092618,24.5010243156706,-15.2589144847989));
#9026=CARTESIAN_POINT('Ctrl Pts',(84.3835320685661,24.0838317927196,-15.2959588574628));
#9027=CARTESIAN_POINT('Ctrl Pts',(84.5702206791894,23.5649502004703,-15.3330032301266));
#9028=CARTESIAN_POINT('Ctrl Pts',(84.7569092898127,23.0460686082211,-15.3700476027905));
#9029=CARTESIAN_POINT('Ctrl Pts',(84.6609637042931,22.4254979466735,-15.4070919754543));
#9030=CARTESIAN_POINT('Ctrl Pts',(84.3262902449012,21.9872235220564,-15.4441363481182));
#9031=CARTESIAN_POINT('Ctrl Pts',(83.9916167855093,21.5489490974392,-15.481180720782));
#9032=CARTESIAN_POINT('Ctrl Pts',(83.418215452245,21.2929709097526,-15.5182250934459));
#9033=CARTESIAN_POINT('Ctrl Pts',(82.8684865098548,21.3364296974664,-15.5552694661097));
#9034=CARTESIAN_POINT('Ctrl Pts',(82.3187575674646,21.3798884851801,-15.5923138387736));
#9035=CARTESIAN_POINT('Ctrl Pts',(81.7927010159485,21.722784248294,-15.6293582114374));
#9036=CARTESIAN_POINT('Ctrl Pts',(81.531049628514,22.20820097358,-15.6664025841013));
#9037=CARTESIAN_POINT('Ctrl Pts',(81.401374715867,22.4487744024699,-15.6847618438643));
#9038=CARTESIAN_POINT('Ctrl Pts',(81.3366433162294,22.7243540007479,-15.7031211036272));
#9039=CARTESIAN_POINT('Ctrl Pts',(81.3367022839223,22.9999597918218,-15.7214803633902));
#9040=CARTESIAN_POINT('Ctrl Pts',(81.3344264707835,23.0015125425552,-15.5285196366098));
#9041=CARTESIAN_POINT('Ctrl Pts',(81.3380786117293,22.5915801840872,-15.501118100834));
#9042=CARTESIAN_POINT('Ctrl Pts',(81.4908760810882,22.1792139742199,-15.4737165650583));
#9043=CARTESIAN_POINT('Ctrl Pts',(81.765275274686,21.8774062461374,-15.4463150292825));
#9044=CARTESIAN_POINT('Ctrl Pts',(82.1362379123091,21.4693897742355,-15.4092706566187));
#9045=CARTESIAN_POINT('Ctrl Pts',(82.7294467853039,21.2634362789804,-15.3722262839548));
#9046=CARTESIAN_POINT('Ctrl Pts',(83.2734377782961,21.3537941624193,-15.335181911291));
#9047=CARTESIAN_POINT('Ctrl Pts',(83.8174287712884,21.4441520458581,-15.2981375386271));
#9048=CARTESIAN_POINT('Ctrl Pts',(84.3122018842782,21.8308213079908,-15.2610931659633));
#9049=CARTESIAN_POINT('Ctrl Pts',(84.5313392342341,22.3368544701007,-15.2240487932994));
#9050=CARTESIAN_POINT('Ctrl Pts',(84.7504765841901,22.8428876322106,-15.1870044206355));
#9051=CARTESIAN_POINT('Ctrl Pts',(84.6939781711122,23.4682846942976,-15.1499600479717));
#9052=CARTESIAN_POINT('Ctrl Pts',(84.3876987654037,23.9268516604712,-15.1129156753078));
#9053=CARTESIAN_POINT('Ctrl Pts',(84.0814193596952,24.3854186266448,-15.075871302644));
#9054=CARTESIAN_POINT('Ctrl Pts',(83.5253589613561,24.677155496905,-15.0388269299801));
#9055=CARTESIAN_POINT('Ctrl Pts',(82.9739817594994,24.6685577343773,-15.0017825573163));
#9056=CARTESIAN_POINT('Ctrl Pts',(82.4226045576427,24.6599599718496,-14.9647381846524));
#9057=CARTESIAN_POINT('Ctrl Pts',(81.8759105522683,24.3510275765339,-14.9276938119886));
#9058=CARTESIAN_POINT('Ctrl Pts',(81.5840776752226,23.8831340941212,-14.8906494393247));
#9059=CARTESIAN_POINT('Ctrl Pts',(81.4209263176052,23.6215547352472,-14.8699395050864));
#9060=CARTESIAN_POINT('Ctrl Pts',(81.3374306038022,23.3102928382113,-14.8492295708481));
#9061=CARTESIAN_POINT('Ctrl Pts',(81.3365468042549,22.999471848124,-14.8285196366098));
#9062=CARTESIAN_POINT('Origin',(83.,23.,-12.));
#9063=CARTESIAN_POINT('',(81.3324917645664,22.9987669698696,-14.1285196366098));
#9064=CARTESIAN_POINT('',(81.3319380765938,23.0009590763004,-14.3214803633902));
#9065=CARTESIAN_POINT('',(81.334,23.,-12.));
#9066=CARTESIAN_POINT('Ctrl Pts',(81.3319380765938,23.0009590763004,-14.3214803633902));
#9067=CARTESIAN_POINT('Ctrl Pts',(81.3315519766315,23.0572154733417,-14.3252552983277));
#9068=CARTESIAN_POINT('Ctrl Pts',(81.3341512946454,23.1134357699009,-14.3290302332651));
#9069=CARTESIAN_POINT('Ctrl Pts',(81.3398536357379,23.1693395494696,-14.3328051682026));
#9070=CARTESIAN_POINT('Ctrl Pts',(81.3958121229659,23.7179372016065,-14.3698495408664));
#9071=CARTESIAN_POINT('Ctrl Pts',(81.7505912237274,24.2360543194683,-14.4068939135303));
#9072=CARTESIAN_POINT('Ctrl Pts',(82.2418370400616,24.4865903135586,-14.4439382861942));
#9073=CARTESIAN_POINT('Ctrl Pts',(82.7330828563959,24.7371263076488,-14.480982658858));
#9074=CARTESIAN_POINT('Ctrl Pts',(83.3607953883029,24.7200811779674,-14.5180270315219));
#9075=CARTESIAN_POINT('Ctrl Pts',(83.8377210268577,24.4432551111368,-14.5550714041857));
#9076=CARTESIAN_POINT('Ctrl Pts',(84.3146466654126,24.1664290443063,-14.5921157768496));
#9077=CARTESIAN_POINT('Ctrl Pts',(84.6407854106153,23.6298220403266,-14.6291601495134));
#9078=CARTESIAN_POINT('Ctrl Pts',(84.6668897564314,23.0789960248702,-14.6662045221773));
#9079=CARTESIAN_POINT('Ctrl Pts',(84.6929941022474,22.5281700094137,-14.7032488948411));
#9080=CARTESIAN_POINT('Ctrl Pts',(84.4190640486767,21.9631249824804,-14.740293267505));
#9081=CARTESIAN_POINT('Ctrl Pts',(83.9704553748996,21.642436667718,-14.7773376401688));
#9082=CARTESIAN_POINT('Ctrl Pts',(83.5218467011226,21.3217483529555,-14.8143820128327));
#9083=CARTESIAN_POINT('Ctrl Pts',(82.8985594071392,21.245416750364,-14.8514263854965));
#9084=CARTESIAN_POINT('Ctrl Pts',(82.385822033276,21.4483727047864,-14.8884707581604));
#9085=CARTESIAN_POINT('Ctrl Pts',(81.8730846594129,21.6513286592087,-14.9255151308242));
#9086=CARTESIAN_POINT('Ctrl Pts',(81.47089720567,22.1335721706451,-14.9625595034881));
#9087=CARTESIAN_POINT('Ctrl Pts',(81.3633085490485,22.6744191151978,-14.9996038761519));
#9088=CARTESIAN_POINT('Ctrl Pts',(81.3421297868928,22.7808845099802,-15.0068960385647));
#9089=CARTESIAN_POINT('Ctrl Pts',(81.33236663533,22.8896207693363,-15.0141882009774));
#9090=CARTESIAN_POINT('Ctrl Pts',(81.333366306688,22.9985354187012,-15.0214803633902));
#9091=CARTESIAN_POINT('Ctrl Pts',(81.3365468042549,22.999471848124,-14.8285196366098));
#9092=CARTESIAN_POINT('Ctrl Pts',(81.3358497296471,22.754319629603,-14.8121851981843));
#9093=CARTESIAN_POINT('Ctrl Pts',(81.3865444352782,22.5094416934687,-14.7958507597587));
#9094=CARTESIAN_POINT('Ctrl Pts',(81.4900814308096,22.2894313720426,-14.7795163213332));
#9095=CARTESIAN_POINT('Ctrl Pts',(81.7248898121595,21.7904767018865,-14.7424719486693));
#9096=CARTESIAN_POINT('Ctrl Pts',(82.2314783235764,21.419421931084,-14.7054275760055));
#9097=CARTESIAN_POINT('Ctrl Pts',(82.7780220917042,21.3460690255097,-14.6683832033416));
#9098=CARTESIAN_POINT('Ctrl Pts',(83.324565859832,21.2727161199355,-14.6313388306778));
#9099=CARTESIAN_POINT('Ctrl Pts',(83.9110648846709,21.4970650795895,-14.5942944580139));
#9100=CARTESIAN_POINT('Ctrl Pts',(84.2691256707508,21.9164494051546,-14.5572500853501));
#9101=CARTESIAN_POINT('Ctrl Pts',(84.6271864568307,22.3358337307197,-14.5202057126862));
#9102=CARTESIAN_POINT('Ctrl Pts',(84.7568090041518,22.9502534221959,-14.4831613400223));
#9103=CARTESIAN_POINT('Ctrl Pts',(84.59867548387,23.4785379372198,-14.4461169673585));
#9104=CARTESIAN_POINT('Ctrl Pts',(84.4405419635882,24.0068224522436,-14.4090725946946));
#9105=CARTESIAN_POINT('Ctrl Pts',(83.9946523757037,24.4489717908152,-14.3720282220308));
#9106=CARTESIAN_POINT('Ctrl Pts',(83.4650545707756,24.6026497141309,-14.3349838493669));
#9107=CARTESIAN_POINT('Ctrl Pts',(82.9354567658475,24.7563276374466,-14.2979394767031));
#9108=CARTESIAN_POINT('Ctrl Pts',(82.3221507438759,24.6215341455064,-14.2608951040392));
#9109=CARTESIAN_POINT('Ctrl Pts',(81.9057974101989,24.2599533929618,-14.2238507313754));
#9110=CARTESIAN_POINT('Ctrl Pts',(81.5486453764393,23.949785824471,-14.1920736997868));
#9111=CARTESIAN_POINT('Ctrl Pts',(81.3364185984152,23.4727395907271,-14.1602966681983));
#9112=CARTESIAN_POINT('Ctrl Pts',(81.3324917645664,22.9987669698696,-14.1285196366098));
#9113=CARTESIAN_POINT('Origin',(83.,23.,-12.));
#9114=CARTESIAN_POINT('',(81.3327117051948,23.0013103746205,-13.4285196366098));
#9115=CARTESIAN_POINT('',(81.3362661788622,23.0008554997906,-13.6214803633902));
#9116=CARTESIAN_POINT('',(81.334,23.,-12.));
#9117=CARTESIAN_POINT('Ctrl Pts',(81.3362661788622,23.0008554997906,-13.6214803633902));
#9118=CARTESIAN_POINT('Ctrl Pts',(81.335230124389,23.2235153031014,-13.6363223956779));
#9119=CARTESIAN_POINT('Ctrl Pts',(81.376782669324,23.4458042723491,-13.6511644279656));
#9120=CARTESIAN_POINT('Ctrl Pts',(81.4627523219824,23.6493315104454,-13.6660064602532));
#9121=CARTESIAN_POINT('Ctrl Pts',(81.6773248137497,24.157317122466,-13.7030508329171));
#9122=CARTESIAN_POINT('Ctrl Pts',(82.1685965800531,24.5484253044889,-13.740095205581));
#9123=CARTESIAN_POINT('Ctrl Pts',(82.7117519925065,24.6436772554877,-13.7771395782448));
#9124=CARTESIAN_POINT('Ctrl Pts',(83.2549074049598,24.7389292064865,-13.8141839509087));
#9125=CARTESIAN_POINT('Ctrl Pts',(83.8499464635632,24.5383249264613,-13.8512283235725));
#9126=CARTESIAN_POINT('Ctrl Pts',(84.2245675848282,24.1336648818027,-13.8882726962364));
#9127=CARTESIAN_POINT('Ctrl Pts',(84.5991887060932,23.729004837144,-13.9253170689002));
#9128=CARTESIAN_POINT('Ctrl Pts',(84.7533918900198,23.120289027852,-13.9623614415641));
#9129=CARTESIAN_POINT('Ctrl Pts',(84.6166107249878,22.5860777876742,-13.9994058142279));
#9130=CARTESIAN_POINT('Ctrl Pts',(84.4798295599558,22.0518665474965,-14.0364501868918));
#9131=CARTESIAN_POINT('Ctrl Pts',(84.0520640459651,21.592159876433,-14.0734945595556));
#9132=CARTESIAN_POINT('Ctrl Pts',(83.5290681004942,21.4173285940911,-14.1105389322195));
#9133=CARTESIAN_POINT('Ctrl Pts',(83.0060721550232,21.2424973117493,-14.1475833048833));
#9134=CARTESIAN_POINT('Ctrl Pts',(82.3878457780718,21.352541418129,-14.1846276775472));
#9135=CARTESIAN_POINT('Ctrl Pts',(81.9573015264435,21.6971025645249,-14.221672050211));
#9136=CARTESIAN_POINT('Ctrl Pts',(81.5706310516055,22.0065518756786,-14.2549414879374));
#9137=CARTESIAN_POINT('Ctrl Pts',(81.3353408713083,22.5051574985021,-14.2882109256638));
#9138=CARTESIAN_POINT('Ctrl Pts',(81.3319380765938,23.0009590763004,-14.3214803633902));
#9139=CARTESIAN_POINT('Ctrl Pts',(81.3324917645664,22.9987669698696,-14.1285196366098));
#9140=CARTESIAN_POINT('Ctrl Pts',(81.3318408550197,22.9202015617864,-14.1232522955345));
#9141=CARTESIAN_POINT('Ctrl Pts',(81.3369132306244,22.8417206048205,-14.1179849544591));
#9142=CARTESIAN_POINT('Ctrl Pts',(81.3479975271719,22.7640981352866,-14.1127176133838));
#9143=CARTESIAN_POINT('Ctrl Pts',(81.4259516232043,22.218191643305,-14.07567324072));
#9144=CARTESIAN_POINT('Ctrl Pts',(81.8012604606514,21.7147466724909,-14.0386288680561));
#9145=CARTESIAN_POINT('Ctrl Pts',(82.3021753294762,21.4841495491966,-14.0015844953923));
#9146=CARTESIAN_POINT('Ctrl Pts',(82.803090198301,21.2535524259023,-13.9645401227284));
#9147=CARTESIAN_POINT('Ctrl Pts',(83.4296110985035,21.295803150128,-13.9274957500645));
#9148=CARTESIAN_POINT('Ctrl Pts',(83.8950297363476,21.5915669589779,-13.8904513774007));
#9149=CARTESIAN_POINT('Ctrl Pts',(84.3604483741916,21.887330767828,-13.8534070047368));
#9150=CARTESIAN_POINT('Ctrl Pts',(84.6647647496773,22.4366076613023,-13.816362632073));
#9151=CARTESIAN_POINT('Ctrl Pts',(84.6687177004905,22.9880377232852,-13.7793182594091));
#9152=CARTESIAN_POINT('Ctrl Pts',(84.6726706513036,23.539467785268,-13.7422738867453));
#9153=CARTESIAN_POINT('Ctrl Pts',(84.3762601774443,24.0930510157592,-13.7052295140814));
#9154=CARTESIAN_POINT('Ctrl Pts',(83.9151295450538,24.3954568340733,-13.6681851414176));
#9155=CARTESIAN_POINT('Ctrl Pts',(83.4539989126633,24.6978626523874,-13.6311407687537));
#9156=CARTESIAN_POINT('Ctrl Pts',(82.8281481217416,24.7490910585245,-13.5940963960899));
#9157=CARTESIAN_POINT('Ctrl Pts',(82.323978810837,24.5256989256713,-13.557052023426));
#9158=CARTESIAN_POINT('Ctrl Pts',(81.8198094999325,24.3023067928182,-13.5200076507622));
#9159=CARTESIAN_POINT('Ctrl Pts',(81.437321669045,23.804294120975,-13.4829632780983));
#9160=CARTESIAN_POINT('Ctrl Pts',(81.3515492768764,23.2595613095707,-13.4459189054345));
#9161=CARTESIAN_POINT('Ctrl Pts',(81.3381205444153,23.1742766276097,-13.4401191491596));
#9162=CARTESIAN_POINT('Ctrl Pts',(81.3319648379856,23.0878467514766,-13.4343193928847));
#9163=CARTESIAN_POINT('Ctrl Pts',(81.3327117051948,23.0013103746205,-13.4285196366098));
#9164=CARTESIAN_POINT('Origin',(83.,23.,-12.));
#9165=CARTESIAN_POINT('',(81.3366135456033,23.0004031163987,-12.7285196366098));
#9166=CARTESIAN_POINT('',(81.3350588241434,22.9985780810801,-12.9214803633902));
#9167=CARTESIAN_POINT('',(81.334,23.,-12.));
#9168=CARTESIAN_POINT('Ctrl Pts',(81.3350588241434,22.9985780810801,-12.9214803633902));
#9169=CARTESIAN_POINT('Ctrl Pts',(81.338211023598,23.3865574103556,-12.9473894930281));
#9170=CARTESIAN_POINT('Ctrl Pts',(81.4733906618918,23.7765167665672,-12.973298622666));
#9171=CARTESIAN_POINT('Ctrl Pts',(81.7211702184837,24.0720803253201,-12.9992077523039));
#9172=CARTESIAN_POINT('Ctrl Pts',(82.0754406382609,24.4946713875952,-13.0362521249677));
#9173=CARTESIAN_POINT('Ctrl Pts',(82.6598960034212,24.7242916927789,-13.0732964976316));
#9174=CARTESIAN_POINT('Ctrl Pts',(83.2070780368979,24.6558624703356,-13.1103408702954));
#9175=CARTESIAN_POINT('Ctrl Pts',(83.7542600703746,24.5874332478923,-13.1473852429593));
#9176=CARTESIAN_POINT('Ctrl Pts',(84.2641687721677,24.2209544978219,-13.1844296156232));
#9177=CARTESIAN_POINT('Ctrl Pts',(84.503459885431,23.7241341083882,-13.221473988287));
#9178=CARTESIAN_POINT('Ctrl Pts',(84.7427509986944,23.2273137189545,-13.2585183609509));
#9179=CARTESIAN_POINT('Ctrl Pts',(84.7114245234279,22.6001516901575,-13.2955627336147));
#9180=CARTESIAN_POINT('Ctrl Pts',(84.4238160712131,22.1296497088031,-13.3326071062786));
#9181=CARTESIAN_POINT('Ctrl Pts',(84.1362076189983,21.6591477274488,-13.3696514789424));
#9182=CARTESIAN_POINT('Ctrl Pts',(83.5923171898351,21.3453057935372,-13.4066958516063));
#9183=CARTESIAN_POINT('Ctrl Pts',(83.0410397477669,21.3317441523751,-13.4437402242701));
#9184=CARTESIAN_POINT('Ctrl Pts',(82.4897623056988,21.3181825112131,-13.480784596934));
#9185=CARTESIAN_POINT('Ctrl Pts',(81.9310978507256,21.6049011628006,-13.5178289695978));
#9186=CARTESIAN_POINT('Ctrl Pts',(81.6207022318547,22.0606920096035,-13.5548733422617));
#9187=CARTESIAN_POINT('Ctrl Pts',(81.4346683301881,22.3338677389618,-13.5770756826379));
#9188=CARTESIAN_POINT('Ctrl Pts',(81.3378160228199,22.6677765355771,-13.599278023014));
#9189=CARTESIAN_POINT('Ctrl Pts',(81.3362661788622,23.0008554997906,-13.6214803633902));
#9190=CARTESIAN_POINT('Ctrl Pts',(81.3327117051948,23.0013103746205,-13.4285196366098));
#9191=CARTESIAN_POINT('Ctrl Pts',(81.3367352500372,22.5351190778817,-13.3972750202208));
#9192=CARTESIAN_POINT('Ctrl Pts',(81.5410869333838,22.0658368917593,-13.3660304038319));
#9193=CARTESIAN_POINT('Ctrl Pts',(81.8878467271069,21.7558629667172,-13.3347857874429));
#9194=CARTESIAN_POINT('Ctrl Pts',(82.2989735229558,21.3883503862333,-13.297741414779));
#9195=CARTESIAN_POINT('Ctrl Pts',(82.9102840681031,21.244778176231,-13.2606970421152));
#9196=CARTESIAN_POINT('Ctrl Pts',(83.4420306266154,21.3908478054807,-13.2236526694514));
#9197=CARTESIAN_POINT('Ctrl Pts',(83.9737771851276,21.5369174347303,-13.1866082967875));
#9198=CARTESIAN_POINT('Ctrl Pts',(84.4259597570048,21.9726289032321,-13.1495639241236));
#9199=CARTESIAN_POINT('Ctrl Pts',(84.5916506984895,22.4985920682814,-13.1125195514598));
#9200=CARTESIAN_POINT('Ctrl Pts',(84.7573416399743,23.0245552333307,-13.0754751787959));
#9201=CARTESIAN_POINT('Ctrl Pts',(84.6365409510666,23.6407700949276,-13.0384308061321));
#9202=CARTESIAN_POINT('Ctrl Pts',(84.284529404345,24.0652446054149,-13.0013864334682));
#9203=CARTESIAN_POINT('Ctrl Pts',(83.9325178576235,24.4897191159023,-12.9643420608044));
#9204=CARTESIAN_POINT('Ctrl Pts',(83.349295453088,24.7224532752801,-12.9272976881405));
#9205=CARTESIAN_POINT('Ctrl Pts',(82.8017562407592,24.6569433520536,-12.8902533154767));
#9206=CARTESIAN_POINT('Ctrl Pts',(82.2542170284304,24.591433428827,-12.8532089428128));
#9207=CARTESIAN_POINT('Ctrl Pts',(81.7423610083083,24.2276794229961,-12.8161645701489));
#9208=CARTESIAN_POINT('Ctrl Pts',(81.500423568429,23.732142326238,-12.7791201974851));
#9209=CARTESIAN_POINT('Ctrl Pts',(81.390265855086,23.506516918766,-12.76225334386));
#9210=CARTESIAN_POINT('Ctrl Pts',(81.3360654021539,23.2535713441157,-12.7453864902349));
#9211=CARTESIAN_POINT('Ctrl Pts',(81.3366135456033,23.0004031163987,-12.7285196366098));
#9212=CARTESIAN_POINT('Origin',(83.,23.,-12.));
#9213=CARTESIAN_POINT('',(81.3341896407369,22.9984774011262,-12.0285196366098));
#9214=CARTESIAN_POINT('',(81.3312396011681,22.9999810457179,-12.2214803633902));
#9215=CARTESIAN_POINT('',(81.334,23.,-12.));
#9216=CARTESIAN_POINT('Ctrl Pts',(81.3312397054754,22.9999810464341,-12.2214803633902));
#9217=CARTESIAN_POINT('Ctrl Pts',(81.3313322642857,23.5504110986567,-12.2584565903783));
#9218=CARTESIAN_POINT('Ctrl Pts',(81.6304402888706,24.100927338771,-12.2954328173664));
#9219=CARTESIAN_POINT('Ctrl Pts',(82.0923259674676,24.4003177084854,-12.3324090443545));
#9220=CARTESIAN_POINT('Ctrl Pts',(82.5550628825009,24.7002598424202,-12.3694534170184));
#9221=CARTESIAN_POINT('Ctrl Pts',(83.1811779895532,24.7481496235668,-12.4064977896822));
#9222=CARTESIAN_POINT('Ctrl Pts',(83.6841486938121,24.5220717456108,-12.4435421623461));
#9223=CARTESIAN_POINT('Ctrl Pts',(84.1871193980711,24.2959938676547,-12.4805865350099));
#9224=CARTESIAN_POINT('Ctrl Pts',(84.5669456995367,23.795948330596,-12.5176309076738));
#9225=CARTESIAN_POINT('Ctrl Pts',(84.6498116077496,23.250765812993,-12.5546752803376));
#9226=CARTESIAN_POINT('Ctrl Pts',(84.7326775159625,22.70558329539,-12.5917196530015));
#9227=CARTESIAN_POINT('Ctrl Pts',(84.5185830309226,22.1152637972427,-12.6287640256654));
#9228=CARTESIAN_POINT('Ctrl Pts',(84.1055020023226,21.7499491382778,-12.6658083983292));
#9229=CARTESIAN_POINT('Ctrl Pts',(83.6924209737225,21.384634479313,-12.7028527709931));
#9230=CARTESIAN_POINT('Ctrl Pts',(83.0803534015624,21.2443246595305,-12.7398971436569));
#9231=CARTESIAN_POINT('Ctrl Pts',(82.5493934522351,21.3932282137333,-12.7769415163208));
#9232=CARTESIAN_POINT('Ctrl Pts',(82.0184335029077,21.542131767936,-12.8139858889846));
#9233=CARTESIAN_POINT('Ctrl Pts',(81.5685811764133,21.980248696124,-12.8510302616485));
#9234=CARTESIAN_POINT('Ctrl Pts',(81.405697750363,22.5070880699012,-12.8880746343123));
#9235=CARTESIAN_POINT('Ctrl Pts',(81.3567362913465,22.6654517845709,-12.8992098773383));
#9236=CARTESIAN_POINT('Ctrl Pts',(81.3337040697582,22.83183206603,-12.9103451203643));
#9237=CARTESIAN_POINT('Ctrl Pts',(81.3350588241434,22.9985780810801,-12.9214803633902));
#9238=CARTESIAN_POINT('Ctrl Pts',(81.3366135456033,23.0004031163987,-12.7285196366098));
#9239=CARTESIAN_POINT('Ctrl Pts',(81.3372692799288,22.6975424377975,-12.708342117571));
#9240=CARTESIAN_POINT('Ctrl Pts',(81.4162752610685,22.3943631223019,-12.6881645985323));
#9241=CARTESIAN_POINT('Ctrl Pts',(81.5715622690257,22.1372558266083,-12.6679870794936));
#9242=CARTESIAN_POINT('Ctrl Pts',(81.8566572691383,21.6652266114217,-12.6309427068297));
#9243=CARTESIAN_POINT('Ctrl Pts',(82.3988661289997,21.3484883687338,-12.5938983341658));
#9244=CARTESIAN_POINT('Ctrl Pts',(82.9500634037713,21.3319867517464,-12.556853961502));
#9245=CARTESIAN_POINT('Ctrl Pts',(83.5012606785428,21.315485134759,-12.5198095888381));
#9246=CARTESIAN_POINT('Ctrl Pts',(84.0614463682244,21.599220143472,-12.4827652161743));
#9247=CARTESIAN_POINT('Ctrl Pts',(84.3742684768708,22.0533490540479,-12.4457208435104));
#9248=CARTESIAN_POINT('Ctrl Pts',(84.687090585517,22.5074779646238,-12.4086764708466));
#9249=CARTESIAN_POINT('Ctrl Pts',(84.7525491131281,23.1320007770625,-12.3716320981827));
#9250=CARTESIAN_POINT('Ctrl Pts',(84.5406889492579,23.6411235619029,-12.3345877255189));
#9251=CARTESIAN_POINT('Ctrl Pts',(84.3288287853876,24.1502463467433,-12.297543352855));
#9252=CARTESIAN_POINT('Ctrl Pts',(83.8396499300361,24.5439691039855,-12.2604989801912));
#9253=CARTESIAN_POINT('Ctrl Pts',(83.2970102543581,24.6421165515269,-12.2234546075273));
#9254=CARTESIAN_POINT('Ctrl Pts',(82.7543705786802,24.7402639990683,-12.1864102348635));
#9255=CARTESIAN_POINT('Ctrl Pts',(82.1582700826758,24.5428361369091,-12.1493658621996));
#9256=CARTESIAN_POINT('Ctrl Pts',(81.7814960844601,24.1401798401158,-12.1123214895357));
#9257=CARTESIAN_POINT('Ctrl Pts',(81.4973831237566,23.8365498837768,-12.0843875385604));
#9258=CARTESIAN_POINT('Ctrl Pts',(81.3379830543993,23.4162234419347,-12.0564535875851));
#9259=CARTESIAN_POINT('Ctrl Pts',(81.3341896407369,22.9984774011262,-12.0285196366098));
#9260=CARTESIAN_POINT('Origin',(83.,23.,-12.));
#9261=CARTESIAN_POINT('',(81.3314456081428,23.0005306221462,-11.3285196366098));
#9262=CARTESIAN_POINT('',(81.335003566498,23.0014338851118,-11.5214803633902));
#9263=CARTESIAN_POINT('',(81.334,23.,-12.));
#9264=CARTESIAN_POINT('Ctrl Pts',(81.335003566498,23.0014338851118,-11.5214803633902));
#9265=CARTESIAN_POINT('Ctrl Pts',(81.3336508586925,23.1661251583794,-11.5324793150647));
#9266=CARTESIAN_POINT('Ctrl Pts',(81.3561117067033,23.3304556252146,-11.5434782667392));
#9267=CARTESIAN_POINT('Ctrl Pts',(81.4038994824931,23.4870574627757,-11.5544772184136));
#9268=CARTESIAN_POINT('Ctrl Pts',(81.5648482917547,24.0144910766468,-11.5915215910775));
#9269=CARTESIAN_POINT('Ctrl Pts',(82.0130896834685,24.4542560288336,-11.6285659637413));
#9270=CARTESIAN_POINT('Ctrl Pts',(82.5434995754815,24.6051072227256,-11.6656103364052));
#9271=CARTESIAN_POINT('Ctrl Pts',(83.0739094674945,24.7559584166175,-11.702654709069));
#9272=CARTESIAN_POINT('Ctrl Pts',(83.6864878598067,24.6178958522146,-11.7396990817329));
#9273=CARTESIAN_POINT('Ctrl Pts',(84.1009068246708,24.2540996760324,-11.7767434543967));
#9274=CARTESIAN_POINT('Ctrl Pts',(84.515325789535,23.8903034998501,-11.8137878270606));
#9275=CARTESIAN_POINT('Ctrl Pts',(84.731585326951,23.3007737118886,-11.8508321997244));
#9276=CARTESIAN_POINT('Ctrl Pts',(84.6507208166511,22.7552907449521,-11.8878765723883));
#9277=CARTESIAN_POINT('Ctrl Pts',(84.5698563063513,22.2098077780156,-11.9249209450521));
#9278=CARTESIAN_POINT('Ctrl Pts',(84.1918677483354,21.7083716321042,-11.961965317716));
#9279=CARTESIAN_POINT('Ctrl Pts',(83.689730145494,21.4804493557541,-11.9990096903798));
#9280=CARTESIAN_POINT('Ctrl Pts',(83.1875925426527,21.2525270794039,-12.0360540630437));
#9281=CARTESIAN_POINT('Ctrl Pts',(82.5613058949858,21.2981186726152,-12.0730984357076));
#9282=CARTESIAN_POINT('Ctrl Pts',(82.0974712976668,21.5963605251005,-12.1101428083714));
#9283=CARTESIAN_POINT('Ctrl Pts',(81.6327834446495,21.8951510140213,-12.147255326711));
#9284=CARTESIAN_POINT('Ctrl Pts',(81.3311468055007,22.4475221540126,-12.1843678450506));
#9285=CARTESIAN_POINT('Ctrl Pts',(81.3312397054754,22.9999810464341,-12.2214803633902));
#9286=CARTESIAN_POINT('Ctrl Pts',(81.3341896407369,22.9984774011262,-12.0285196366098));
#9287=CARTESIAN_POINT('Ctrl Pts',(81.3329524509769,22.8622330655561,-12.0194092149213));
#9288=CARTESIAN_POINT('Ctrl Pts',(81.3482668769255,22.7262632028618,-12.0102987932327));
#9289=CARTESIAN_POINT('Ctrl Pts',(81.381204657911,22.5947056619895,-12.0011883715442));
#9290=CARTESIAN_POINT('Ctrl Pts',(81.5151347300046,22.0597725120841,-11.9641439988803));
#9291=CARTESIAN_POINT('Ctrl Pts',(81.9404423746189,21.5977909437006,-11.9270996262165));
#9292=CARTESIAN_POINT('Ctrl Pts',(82.4624984436055,21.4201728142401,-11.8900552535526));
#9293=CARTESIAN_POINT('Ctrl Pts',(82.9845545125921,21.2425546847796,-11.8530108808888));
#9294=CARTESIAN_POINT('Ctrl Pts',(83.603359005951,21.3492999942421,-11.8159665082249));
#9295=CARTESIAN_POINT('Ctrl Pts',(84.0357348095674,21.6915599882903,-11.7789221355611));
#9296=CARTESIAN_POINT('Ctrl Pts',(84.4681106131838,22.0338199823385,-11.7418777628972));
#9297=CARTESIAN_POINT('Ctrl Pts',(84.7140577270577,22.6115946609723,-11.7048333902334));
#9298=CARTESIAN_POINT('Ctrl Pts',(84.6610259116884,23.1604829607542,-11.6677890175695));
#9299=CARTESIAN_POINT('Ctrl Pts',(84.607994096319,23.709371260536,-11.6307446449057));
#9300=CARTESIAN_POINT('Ctrl Pts',(84.2559833517065,24.2293731814658,-11.5937002722418));
#9301=CARTESIAN_POINT('Ctrl Pts',(83.7660807220893,24.4825256109881,-11.5566558995779));
#9302=CARTESIAN_POINT('Ctrl Pts',(83.2761780924722,24.7356780405103,-11.5196115269141));
#9303=CARTESIAN_POINT('Ctrl Pts',(82.6483835778505,24.7219809786249,-11.4825671542502));
#9304=CARTESIAN_POINT('Ctrl Pts',(82.1699883029908,24.4477024704062,-11.4455227815864));
#9305=CARTESIAN_POINT('Ctrl Pts',(81.6915930281311,24.1734239621876,-11.4084784089225));
#9306=CARTESIAN_POINT('Ctrl Pts',(81.3625969930333,23.6385640076356,-11.3714340362587));
#9307=CARTESIAN_POINT('Ctrl Pts',(81.3335552579371,23.0878850478946,-11.3343896635948));
#9308=CARTESIAN_POINT('Ctrl Pts',(81.3320212798414,23.0587983056868,-11.3324329879332));
#9309=CARTESIAN_POINT('Ctrl Pts',(81.3313241530342,23.029667429573,-11.3304763122715));
#9310=CARTESIAN_POINT('Ctrl Pts',(81.3314456081428,23.0005306221462,-11.3285196366098));
#9311=CARTESIAN_POINT('Origin',(83.,23.,-12.));
#9312=CARTESIAN_POINT('',(81.3357537722937,23.0011866319928,-10.6285196366098));
#9313=CARTESIAN_POINT('',(81.3362973248117,22.9991726428529,-10.8214803633902));
#9314=CARTESIAN_POINT('',(81.334,23.,-12.));
#9315=CARTESIAN_POINT('Ctrl Pts',(81.3362973248117,22.9991726428529,-10.8214803633902));
#9316=CARTESIAN_POINT('Ctrl Pts',(81.3377853361398,23.3302224779932,-10.8435464124149));
#9317=CARTESIAN_POINT('Ctrl Pts',(81.4333699684559,23.6620640474109,-10.8656124614396));
#9318=CARTESIAN_POINT('Ctrl Pts',(81.6172642260941,23.9342395911072,-10.8876785104643));
#9319=CARTESIAN_POINT('Ctrl Pts',(81.9259849854412,24.391166531648,-10.9247228831281));
#9320=CARTESIAN_POINT('Ctrl Pts',(82.4835934100557,24.6799335713466,-10.961767255792));
#9321=CARTESIAN_POINT('Ctrl Pts',(83.0349169112071,24.668395229957,-10.9988116284558));
#9322=CARTESIAN_POINT('Ctrl Pts',(83.5862404123585,24.6568568885673,-11.0358560011197));
#9323=CARTESIAN_POINT('Ctrl Pts',(84.1312789900469,24.3450131660894,-11.0729003737835));
#9324=CARTESIAN_POINT('Ctrl Pts',(84.4206122648672,23.8755698869538,-11.1099447464474));
#9325=CARTESIAN_POINT('Ctrl Pts',(84.7099455396876,23.4061266078182,-11.1469891191112));
#9326=CARTESIAN_POINT('Ctrl Pts',(84.74357351164,22.7790837720248,-11.1840334917751));
#9327=CARTESIAN_POINT('Ctrl Pts',(84.5061073589669,22.2813885213156,-11.2210778644389));
#9328=CARTESIAN_POINT('Ctrl Pts',(84.2686412062939,21.7836932706063,-11.2581222371028));
#9329=CARTESIAN_POINT('Ctrl Pts',(83.7600809289955,21.4153456049811,-11.2951666097666));
#9330=CARTESIAN_POINT('Ctrl Pts',(83.2131537183322,21.3449086652415,-11.3322109824305));
#9331=CARTESIAN_POINT('Ctrl Pts',(82.6662265076688,21.2744717255019,-11.3692553550943));
#9332=CARTESIAN_POINT('Ctrl Pts',(82.0809323636405,21.5019455116479,-11.4062997277582));
#9333=CARTESIAN_POINT('Ctrl Pts',(81.7251134050312,21.9232335424986,-11.4433441004221));
#9334=CARTESIAN_POINT('Ctrl Pts',(81.4749416810535,22.2194357273989,-11.4693895214114));
#9335=CARTESIAN_POINT('Ctrl Pts',(81.3382067667041,22.6114463960778,-11.4954349424008));
#9336=CARTESIAN_POINT('Ctrl Pts',(81.335003566498,23.0014338851118,-11.5214803633902));
#9337=CARTESIAN_POINT('Ctrl Pts',(81.3314456081428,23.0005306221462,-11.3285196366098));
#9338=CARTESIAN_POINT('Ctrl Pts',(81.3336235777125,22.4780406200363,-11.2934319396076));
#9339=CARTESIAN_POINT('Ctrl Pts',(81.5990308224674,21.953643300933,-11.2583442426054));
#9340=CARTESIAN_POINT('Ctrl Pts',(82.0223180314453,21.6476317704281,-11.2232565456033));
#9341=CARTESIAN_POINT('Ctrl Pts',(82.4692099751442,21.3245554176324,-11.1862121729394));
#9342=CARTESIAN_POINT('Ctrl Pts',(83.0920812976368,21.244900676971,-11.1491678002756));
#9343=CARTESIAN_POINT('Ctrl Pts',(83.605893823762,21.4451191253606,-11.1121234276117));
#9344=CARTESIAN_POINT('Ctrl Pts',(84.1197063498873,21.6453375737501,-11.0750790549479));
#9345=CARTESIAN_POINT('Ctrl Pts',(84.5244600796454,22.1254292111906,-11.038034682284));
#9346=CARTESIAN_POINT('Ctrl Pts',(84.6349317408232,22.6656946562779,-11.0009903096202));
#9347=CARTESIAN_POINT('Ctrl Pts',(84.745403402001,23.2059601013652,-10.9639459369563));
#9348=CARTESIAN_POINT('Ctrl Pts',(84.5615929945986,23.8063993540994,-10.9269015642925));
#9349=CARTESIAN_POINT('Ctrl Pts',(84.1676157783968,24.1922395958998,-10.8898571916286));
#9350=CARTESIAN_POINT('Ctrl Pts',(83.7736385621949,24.5780798377003,-10.8528128189648));
#9351=CARTESIAN_POINT('Ctrl Pts',(83.1694945371938,24.7493210685671,-10.8157684463009));
#9352=CARTESIAN_POINT('Ctrl Pts',(82.6316518986724,24.627599931261,-10.778724073637));
#9353=CARTESIAN_POINT('Ctrl Pts',(82.093809260151,24.5058787939549,-10.7416797009732));
#9354=CARTESIAN_POINT('Ctrl Pts',(81.6222680081092,24.0911952884759,-10.7046353283093));
#9355=CARTESIAN_POINT('Ctrl Pts',(81.432814699323,23.573316747823,-10.6675909556455));
#9356=CARTESIAN_POINT('Ctrl Pts',(81.3662081755097,23.3912450301455,-10.6545671826336));
#9357=CARTESIAN_POINT('Ctrl Pts',(81.3344685786651,23.1964180925411,-10.6415434096217));
#9358=CARTESIAN_POINT('Ctrl Pts',(81.3357537722937,23.0011866319928,-10.6285196366098));
#9359=CARTESIAN_POINT('Origin',(83.,23.,-12.));
#9360=CARTESIAN_POINT('',(81.3357306082006,22.9988024506805,-9.92851963660979));
#9361=CARTESIAN_POINT('',(81.3319839553715,22.9990126570311,-10.1214803633902));
#9362=CARTESIAN_POINT('',(81.334,23.,-12.));
#9363=CARTESIAN_POINT('Ctrl Pts',(81.3319839553715,22.9990126570311,-10.1214803633902));
#9364=CARTESIAN_POINT('Ctrl Pts',(81.3354513145775,23.4928188600527,-10.1546135097651));
#9365=CARTESIAN_POINT('Ctrl Pts',(81.568574055279,23.9894690902029,-10.18774665614));
#9366=CARTESIAN_POINT('Ctrl Pts',(81.9525268672513,24.2990619193099,-10.2208798025149));
#9367=CARTESIAN_POINT('Ctrl Pts',(82.3818036673203,24.6452008584172,-10.2579241751788));
#9368=CARTESIAN_POINT('Ctrl Pts',(82.9996220147768,24.757513137192,-10.2949685478426));
#9369=CARTESIAN_POINT('Ctrl Pts',(83.5232560752779,24.5846024465828,-10.3320129205065));
#9370=CARTESIAN_POINT('Ctrl Pts',(84.0468901357791,24.4116917559736,-10.3690572931703));
#9371=CARTESIAN_POINT('Ctrl Pts',(84.476339909325,23.9535580959804,-10.4061016658342));
#9372=CARTESIAN_POINT('Ctrl Pts',(84.6150807280518,23.4198524453986,-10.443146038498));
#9373=CARTESIAN_POINT('Ctrl Pts',(84.7538215467786,22.8861467948169,-10.4801904111619));
#9374=CARTESIAN_POINT('Ctrl Pts',(84.6018534106864,22.2768691536466,-10.5172347838257));
#9375=CARTESIAN_POINT('Ctrl Pts',(84.2287199295546,21.8708369609544,-10.5542791564896));
#9376=CARTESIAN_POINT('Ctrl Pts',(83.8555864484229,21.4648047682622,-10.5913235291534));
#9377=CARTESIAN_POINT('Ctrl Pts',(83.2612876222518,21.2620180240482,-10.6283679018173));
#9378=CARTESIAN_POINT('Ctrl Pts',(82.717786289584,21.3552759332688,-10.6654122744811));
#9379=CARTESIAN_POINT('Ctrl Pts',(82.1742849569162,21.4485338424895,-10.702456647145));
#9380=CARTESIAN_POINT('Ctrl Pts',(81.6815811177517,21.8378364051449,-10.7395010198088));
#9381=CARTESIAN_POINT('Ctrl Pts',(81.4651457452094,22.3450311071641,-10.7765453924727));
#9382=CARTESIAN_POINT('Ctrl Pts',(81.3776334235319,22.5501075020015,-10.7915237161119));
#9383=CARTESIAN_POINT('Ctrl Pts',(81.3352872701694,22.7744576716372,-10.806502039751));
#9384=CARTESIAN_POINT('Ctrl Pts',(81.3362973248117,22.9991726428529,-10.8214803633902));
#9385=CARTESIAN_POINT('Ctrl Pts',(81.3357537722937,23.0011866319928,-10.6285196366098));
#9386=CARTESIAN_POINT('Ctrl Pts',(81.3381241392834,22.6411084312276,-10.6044990369578));
#9387=CARTESIAN_POINT('Ctrl Pts',(81.4528344298303,22.2796541709646,-10.5804784373059));
#9388=CARTESIAN_POINT('Ctrl Pts',(81.6683271709657,21.9943115112502,-10.5564578376539));
#9389=CARTESIAN_POINT('Ctrl Pts',(82.0006583169253,21.5542583911568,-10.5194134649901));
#9390=CARTESIAN_POINT('Ctrl Pts',(82.5726859743754,21.2952257267967,-10.4823690923262));
#9391=CARTESIAN_POINT('Ctrl Pts',(83.1226390298723,21.3357519630943,-10.4453247196624));
#9392=CARTESIAN_POINT('Ctrl Pts',(83.6725920853691,21.3762781993919,-10.4082803469985));
#9393=CARTESIAN_POINT('Ctrl Pts',(84.2004705389127,21.7163633363471,-10.3712359743347));
#9394=CARTESIAN_POINT('Ctrl Pts',(84.4647068216147,22.200377722479,-10.3341916016708));
#9395=CARTESIAN_POINT('Ctrl Pts',(84.7289431043167,22.6843921086108,-10.297147229007));
#9396=CARTESIAN_POINT('Ctrl Pts',(84.7295372161771,23.3123357439193,-10.2601028563431));
#9397=CARTESIAN_POINT('Ctrl Pts',(84.4662172799166,23.796849263077,-10.2230584836792));
#9398=CARTESIAN_POINT('Ctrl Pts',(84.2028973436561,24.2813627822347,-10.1860141110154));
#9399=CARTESIAN_POINT('Ctrl Pts',(83.6756633592748,24.6224461852415,-10.1489697383515));
#9400=CARTESIAN_POINT('Ctrl Pts',(83.1257879738892,24.6640129944256,-10.1119253656877));
#9401=CARTESIAN_POINT('Ctrl Pts',(82.5759125885035,24.7055798036097,-10.0748809930238));
#9402=CARTESIAN_POINT('Ctrl Pts',(82.0033958021135,24.4476300189711,-10.03783662036));
#9403=CARTESIAN_POINT('Ctrl Pts',(81.6702325631919,24.0082065383626,-10.0007922476961));
#9404=CARTESIAN_POINT('Ctrl Pts',(81.4535682813828,23.7224385972649,-9.97670137733401));
#9405=CARTESIAN_POINT('Ctrl Pts',(81.3381319306509,23.3599213997545,-9.9526105069719));
#9406=CARTESIAN_POINT('Ctrl Pts',(81.3357306082006,22.9988024506805,-9.92851963660979));
#9407=CARTESIAN_POINT('Origin',(83.,23.,-12.));
#9408=CARTESIAN_POINT('',(81.3314317338341,22.9994875421002,-9.22851963660979));
#9409=CARTESIAN_POINT('',(81.3333049749392,23.0014544405517,-9.42148036339021));
#9410=CARTESIAN_POINT('',(81.334,23.,-12.));
#9411=CARTESIAN_POINT('Ctrl Pts',(81.3333049749392,23.0014544405517,-9.42148036339021));
#9412=CARTESIAN_POINT('Ctrl Pts',(81.3323267877789,23.1083233317145,-9.42863623445147));
#9413=CARTESIAN_POINT('Ctrl Pts',(81.34172531431,23.2150208601815,-9.43579210551273));
#9414=CARTESIAN_POINT('Ctrl Pts',(81.362124673025,23.3195719751752,-9.44294797657399));
#9415=CARTESIAN_POINT('Ctrl Pts',(81.4677276722785,23.8608101323596,-9.47999234923784));
#9416=CARTESIAN_POINT('Ctrl Pts',(81.8681425754562,24.3445264373676,-9.5170367219017));
#9417=CARTESIAN_POINT('Ctrl Pts',(82.380131642776,24.5493627895829,-9.55408109456555));
#9418=CARTESIAN_POINT('Ctrl Pts',(82.8921207100958,24.7541991417982,-9.5911254672294));
#9419=CARTESIAN_POINT('Ctrl Pts',(83.5156839415576,24.6801555412208,-9.62816983989325));
#9420=CARTESIAN_POINT('Ctrl Pts',(83.9654665308395,24.361115796639,-9.66521421255711));
#9421=CARTESIAN_POINT('Ctrl Pts',(84.4152491201214,24.0420760520572,-9.70225858522096));
#9422=CARTESIAN_POINT('Ctrl Pts',(84.6912510672232,23.478040163471,-9.73930295788482));
#9423=CARTESIAN_POINT('Ctrl Pts',(84.6671684494862,22.9271220536155,-9.77634733054867));
#9424=CARTESIAN_POINT('Ctrl Pts',(84.643085831749,22.37620394376,-9.81339170321253));
#9425=CARTESIAN_POINT('Ctrl Pts',(84.318918649173,21.8384036126351,-9.85043607587637));
#9426=CARTESIAN_POINT('Ctrl Pts',(83.8430121840525,21.559829075571,-9.88748044854023));
#9427=CARTESIAN_POINT('Ctrl Pts',(83.3671057189321,21.281254538507,-9.92452482120408));
#9428=CARTESIAN_POINT('Ctrl Pts',(82.7394599712673,21.2619057955038,-9.96156919386793));
#9429=CARTESIAN_POINT('Ctrl Pts',(82.2472979871377,21.5106372121392,-9.99861356653178));
#9430=CARTESIAN_POINT('Ctrl Pts',(81.755136003008,21.7593686287746,-10.0356579391956));
#9431=CARTESIAN_POINT('Ctrl Pts',(81.3984577824135,22.2761802050487,-10.0727023118595));
#9432=CARTESIAN_POINT('Ctrl Pts',(81.3404862984571,22.8245687929057,-10.1097466845233));
#9433=CARTESIAN_POINT('Ctrl Pts',(81.3343655417603,22.8824688653634,-10.1136579108123));
#9434=CARTESIAN_POINT('Ctrl Pts',(81.3315746484398,22.9407209457323,-10.1175691371013));
#9435=CARTESIAN_POINT('Ctrl Pts',(81.3319839553715,22.9990126570311,-10.1214803633902));
#9436=CARTESIAN_POINT('Ctrl Pts',(81.3357306082006,22.9988024506805,-9.92851963660979));
#9437=CARTESIAN_POINT('Ctrl Pts',(81.3344394329371,22.8046311705349,-9.91556613430805));
#9438=CARTESIAN_POINT('Ctrl Pts',(81.3658282901416,22.610864143876,-9.90261263200631));
#9439=CARTESIAN_POINT('Ctrl Pts',(81.4317326497978,22.4296497757676,-9.88965912970457));
#9440=CARTESIAN_POINT('Ctrl Pts',(81.6202056667786,21.9114136703591,-9.85261475704072));
#9441=CARTESIAN_POINT('Ctrl Pts',(82.0909613921934,21.4958386361202,-9.81557038437687));
#9442=CARTESIAN_POINT('Ctrl Pts',(82.6285727417101,21.373099987156,-9.77852601171301));
#9443=CARTESIAN_POINT('Ctrl Pts',(83.1661840912268,21.2503613381917,-9.74148163904916));
#9444=CARTESIAN_POINT('Ctrl Pts',(83.7706510648454,21.420459074502,-9.7044372663853));
#9445=CARTESIAN_POINT('Ctrl Pts',(84.1653576796438,21.80555312446,-9.66739289372145));
#9446=CARTESIAN_POINT('Ctrl Pts',(84.5600642944423,22.1906471744179,-9.6303485210576));
#9447=CARTESIAN_POINT('Ctrl Pts',(84.7450105504205,22.7907375380235,-9.59330414839374));
#9448=CARTESIAN_POINT('Ctrl Pts',(84.6355614011362,23.3312110552286,-9.55625977572989));
#9449=CARTESIAN_POINT('Ctrl Pts',(84.5261122518518,23.8716845724337,-9.51921540306604));
#9450=CARTESIAN_POINT('Ctrl Pts',(84.1222676973048,24.3525412432383,-9.48217103040219));
#9451=CARTESIAN_POINT('Ctrl Pts',(83.6088349532393,24.553731591913,-9.44512665773834));
#9452=CARTESIAN_POINT('Ctrl Pts',(83.0954022091738,24.7549219405877,-9.40808228507448));
#9453=CARTESIAN_POINT('Ctrl Pts',(82.4723812755898,24.6764459671325,-9.37103791241063));
#9454=CARTESIAN_POINT('Ctrl Pts',(82.0248787926276,24.3542158213969,-9.33399353974677));
#9455=CARTESIAN_POINT('Ctrl Pts',(81.6001644105017,24.0483945523337,-9.29883557203444));
#9456=CARTESIAN_POINT('Ctrl Pts',(81.3335478235868,23.5230123364042,-9.26367760432212));
#9457=CARTESIAN_POINT('Ctrl Pts',(81.3314317338341,22.9994875421002,-9.22851963660979));
#9458=CARTESIAN_POINT('Origin',(83.,23.,-12.));
#9459=CARTESIAN_POINT('',(81.3342211202573,23.0015219661406,-8.52851963660979));
#9460=CARTESIAN_POINT('',(81.3367006745913,23.0000736897444,-8.72148036339021));
#9461=CARTESIAN_POINT('',(81.334,23.,-12.));
#9462=CARTESIAN_POINT('Ctrl Pts',(81.3367006745913,23.0000736897444,-8.72148036339021));
#9463=CARTESIAN_POINT('Ctrl Pts',(81.3365927347494,23.2736326870282,-8.73970333180169));
#9464=CARTESIAN_POINT('Ctrl Pts',(81.4003184029638,23.5471443306604,-8.75792630021316));
#9465=CARTESIAN_POINT('Ctrl Pts',(81.5281532937941,23.7864026369698,-8.77614926862464));
#9466=CARTESIAN_POINT('Ctrl Pts',(81.7880211280806,24.2727764077912,-8.81319364128849));
#9467=CARTESIAN_POINT('Ctrl Pts',(82.3128162877671,24.6176004191139,-8.85023801395234));
#9468=CARTESIAN_POINT('Ctrl Pts',(82.8623821799344,24.6630764172596,-8.8872823866162));
#9469=CARTESIAN_POINT('Ctrl Pts',(83.4119480721017,24.7085524154054,-8.92432675928005));
#9470=CARTESIAN_POINT('Ctrl Pts',(83.9862846967497,24.4546804003742,-8.9613711319439));
#9471=CARTESIAN_POINT('Ctrl Pts',(84.3225643115941,24.0176372024102,-8.99841550460776));
#9472=CARTESIAN_POINT('Ctrl Pts',(84.6588439264386,23.5805940044462,-9.03545987727161));
#9473=CARTESIAN_POINT('Ctrl Pts',(84.7570665314794,22.9603796235494,-9.07250424993546));
#9474=CARTESIAN_POINT('Ctrl Pts',(84.5722835296534,22.4408163661117,-9.10954862259932));
#9475=CARTESIAN_POINT('Ctrl Pts',(84.3875005278274,21.9212531086739,-9.14659299526317));
#9476=CARTESIAN_POINT('Ctrl Pts',(83.9197119191345,21.5023409746951,-9.18363736792702));
#9477=CARTESIAN_POINT('Ctrl Pts',(83.3829869769,21.3757824007978,-9.22068174059087));
#9478=CARTESIAN_POINT('Ctrl Pts',(82.8462620346654,21.2492238269004,-9.25772611325473));
#9479=CARTESIAN_POINT('Ctrl Pts',(82.2406007588892,21.4150188130846,-9.29477048591858));
#9480=CARTESIAN_POINT('Ctrl Pts',(81.8431656686657,21.7972963108572,-9.33181485858244));
#9481=CARTESIAN_POINT('Ctrl Pts',(81.5225032177487,22.1057291653825,-9.36170336018503));
#9482=CARTESIAN_POINT('Ctrl Pts',(81.3373906478447,22.5550865564124,-9.39159186178762));
#9483=CARTESIAN_POINT('Ctrl Pts',(81.3333049749392,23.0014544405517,-9.42148036339021));
#9484=CARTESIAN_POINT('Ctrl Pts',(81.3314317338341,22.9994875421002,-9.22851963660979));
#9485=CARTESIAN_POINT('Ctrl Pts',(81.331318194786,22.9713977568116,-9.22663323165826));
#9486=CARTESIAN_POINT('Ctrl Pts',(81.3319661187671,22.9433133188019,-9.22474682670673));
#9487=CARTESIAN_POINT('Ctrl Pts',(81.3333919413996,22.9152684297273,-9.22286042175521));
#9488=CARTESIAN_POINT('Ctrl Pts',(81.3613916054742,22.3645355018094,-9.18581604909136));
#9489=CARTESIAN_POINT('Ctrl Pts',(81.6893749659637,21.8290539639894,-9.14877167642751));
#9490=CARTESIAN_POINT('Ctrl Pts',(82.1672503824573,21.5538707061649,-9.11172730376366));
#9491=CARTESIAN_POINT('Ctrl Pts',(82.6451257989509,21.2786874483404,-9.0746829310998));
#9492=CARTESIAN_POINT('Ctrl Pts',(83.2728932714485,21.2638024705112,-9.03763855843595));
#9493=CARTESIAN_POINT('Ctrl Pts',(83.7632740501943,21.5160274314317,-9.00059418577209));
#9494=CARTESIAN_POINT('Ctrl Pts',(84.2536548289401,21.7682523923522,-8.96354981310824));
#9495=CARTESIAN_POINT('Ctrl Pts',(84.606648913934,22.2875872920222,-8.92650544044439));
#9496=CARTESIAN_POINT('Ctrl Pts',(84.6607192650221,22.8363742600094,-8.88946106778053));
#9497=CARTESIAN_POINT('Ctrl Pts',(84.7147896161103,23.3851612279965,-8.85241669511668));
#9498=CARTESIAN_POINT('Ctrl Pts',(84.4699362332925,23.9634002643006,-8.81537232245283));
#9499=CARTESIAN_POINT('Ctrl Pts',(84.0382088432236,24.3064778061407,-8.77832794978898));
#9500=CARTESIAN_POINT('Ctrl Pts',(83.6064814531546,24.6495553479807,-8.74128357712513));
#9501=CARTESIAN_POINT('Ctrl Pts',(82.9878800558344,24.7574713953565,-8.70423920446127));
#9502=CARTESIAN_POINT('Ctrl Pts',(82.4654888246145,24.5808414414913,-8.66719483179742));
#9503=CARTESIAN_POINT('Ctrl Pts',(81.9430975933946,24.4042114876261,-8.63015045913357));
#9504=CARTESIAN_POINT('Ctrl Pts',(81.5169165282749,23.9430355325199,-8.59310608646971));
#9505=CARTESIAN_POINT('Ctrl Pts',(81.381974471854,23.4083567685463,-8.55606171380586));
#9506=CARTESIAN_POINT('Ctrl Pts',(81.3485318347526,23.275847539447,-8.54688102140717));
#9507=CARTESIAN_POINT('Ctrl Pts',(81.3329769563652,23.1388238034631,-8.53770032900848));
#9508=CARTESIAN_POINT('Ctrl Pts',(81.3342211202573,23.0015219661406,-8.52851963660979));
#9509=CARTESIAN_POINT('Origin',(83.,23.,-12.));
#9510=CARTESIAN_POINT('',(81.3366057744099,22.9995801773856,-7.82851963660979));
#9511=CARTESIAN_POINT('',(81.3335754310806,22.9985070363431,-8.02148036339021));
#9512=CARTESIAN_POINT('',(81.334,23.,-12.));
#9513=CARTESIAN_POINT('Ctrl Pts',(81.3335754310806,22.9985070363431,-8.02148036339021));
#9514=CARTESIAN_POINT('Ctrl Pts',(81.3376142783493,23.4361202976576,-8.05077042915191));
#9515=CARTESIAN_POINT('Ctrl Pts',(81.5146048683971,23.8766246058543,-8.08006049491359));
#9516=CARTESIAN_POINT('Ctrl Pts',(81.8239355688047,24.1839063669557,-8.10935056067528));
#9517=CARTESIAN_POINT('Ctrl Pts',(82.2151590585539,24.5725384773669,-8.14639493333913));
#9518=CARTESIAN_POINT('Ctrl Pts',(82.8180700843827,24.7480715305975,-8.18343930600298));
#9519=CARTESIAN_POINT('Ctrl Pts',(83.3567646970391,24.6301781453598,-8.22048367866684));
#9520=CARTESIAN_POINT('Ctrl Pts',(83.8954593096956,24.5122847601222,-8.2575280513307));
#9521=CARTESIAN_POINT('Ctrl Pts',(84.3699375091796,24.1009649364163,-8.29457242399455));
#9522=CARTESIAN_POINT('Ctrl Pts',(84.5630687330952,23.5844467211039,-8.33161679665841));
#9523=CARTESIAN_POINT('Ctrl Pts',(84.7561999570107,23.0679285057914,-8.36866116932226));
#9524=CARTESIAN_POINT('Ctrl Pts',(84.6679842053578,22.4462118988724,-8.4057055419861));
#9525=CARTESIAN_POINT('Ctrl Pts',(84.3387907424989,22.0038066545161,-8.44274991464995));
#9526=CARTESIAN_POINT('Ctrl Pts',(84.0095972796401,21.5614014101598,-8.47979428731381));
#9527=CARTESIAN_POINT('Ctrl Pts',(83.4394261055753,21.2983075283662,-8.51683865997767));
#9528=CARTESIAN_POINT('Ctrl Pts',(82.8891987702469,21.334921947292,-8.55388303264152));
#9529=CARTESIAN_POINT('Ctrl Pts',(82.3389714349186,21.3715363662178,-8.59092740530538));
#9530=CARTESIAN_POINT('Ctrl Pts',(81.8086879383266,21.707859085863,-8.62797177796922));
#9531=CARTESIAN_POINT('Ctrl Pts',(81.5410164444739,22.1899822108456,-8.66501615063307));
#9532=CARTESIAN_POINT('Ctrl Pts',(81.4050186388596,22.4349380187644,-8.68383755488545));
#9533=CARTESIAN_POINT('Ctrl Pts',(81.3368121591394,22.7175311116915,-8.70265895913783));
#9534=CARTESIAN_POINT('Ctrl Pts',(81.3367006745913,23.0000736897444,-8.72148036339021));
#9535=CARTESIAN_POINT('Ctrl Pts',(81.3342211202573,23.0015219661406,-8.52851963660979));
#9536=CARTESIAN_POINT('Ctrl Pts',(81.3379971954574,22.5848067197478,-8.50065595634463));
#9537=CARTESIAN_POINT('Ctrl Pts',(81.4965161259226,22.1655297680809,-8.47279227607946));
#9538=CARTESIAN_POINT('Ctrl Pts',(81.779340767355,21.8621279077235,-8.4449285958143));
#9539=CARTESIAN_POINT('Ctrl Pts',(82.1553521669993,21.4587593837155,-8.40788422315045));
#9540=CARTESIAN_POINT('Ctrl Pts',(82.7510780140101,21.2602039085407,-8.37083985048659));
#9541=CARTESIAN_POINT('Ctrl Pts',(83.293902437176,21.3573243730351,-8.33379547782274));
#9542=CARTESIAN_POINT('Ctrl Pts',(83.836726860342,21.4544448375295,-8.29675110515889));
#9543=CARTESIAN_POINT('Ctrl Pts',(84.3266498596631,21.847241241693,-8.25970673249503));
#9544=CARTESIAN_POINT('Ctrl Pts',(84.5394730287578,22.355962225086,-8.22266235983118));
#9545=CARTESIAN_POINT('Ctrl Pts',(84.7522961978524,22.864683208479,-8.18561798716733));
#9546=CARTESIAN_POINT('Ctrl Pts',(84.6880195367206,23.4893287711015,-8.14857361450347));
#9547=CARTESIAN_POINT('Ctrl Pts',(84.3760573110503,23.9440488020894,-8.11152924183962));
#9548=CARTESIAN_POINT('Ctrl Pts',(84.06409508538,24.3987688330773,-8.07448486917577));
#9549=CARTESIAN_POINT('Ctrl Pts',(83.5044472951711,24.6835633324306,-8.03744049651192));
#9550=CARTESIAN_POINT('Ctrl Pts',(82.9532197817844,24.6681047495028,-8.00039612384807));
#9551=CARTESIAN_POINT('Ctrl Pts',(82.4019922683977,24.6526461665751,-7.96335175118421));
#9552=CARTESIAN_POINT('Ctrl Pts',(81.859185031833,24.3369345013664,-7.92630737852035));
#9553=CARTESIAN_POINT('Ctrl Pts',(81.5731973482785,23.8654455911985,-7.8892630058565));
#9554=CARTESIAN_POINT('Ctrl Pts',(81.416881609315,23.6077382085239,-7.8690152161076));
#9555=CARTESIAN_POINT('Ctrl Pts',(81.3372912138979,23.3034920693719,-7.84876742635869));
#9556=CARTESIAN_POINT('Ctrl Pts',(81.3366057744099,22.9995801773856,-7.82851963660979));
#9557=CARTESIAN_POINT('Origin',(83.,23.,-12.));
#9558=CARTESIAN_POINT('',(81.3326822579993,22.9986976815004,-7.12851963660979));
#9559=CARTESIAN_POINT('',(81.3317908287134,23.0008588708997,-7.32148036339021));
#9560=CARTESIAN_POINT('',(81.334,23.,-12.));
#9561=CARTESIAN_POINT('Ctrl Pts',(81.3317908287134,23.0008588708997,-7.32148036339021));
#9562=CARTESIAN_POINT('Ctrl Pts',(81.3314807791329,23.0502166331272,-7.32479315383826));
#9563=CARTESIAN_POINT('Ctrl Pts',(81.333481500878,23.099548907092,-7.32810594428632));
#9564=CARTESIAN_POINT('Ctrl Pts',(81.3378748305336,23.1486671753356,-7.33141873473437));
#9565=CARTESIAN_POINT('Ctrl Pts',(81.3870020372038,23.6979187691063,-7.36846310739822));
#9566=CARTESIAN_POINT('Ctrl Pts',(81.7353061679567,24.2204106196216,-7.40550748006207));
#9567=CARTESIAN_POINT('Ctrl Pts',(82.2233962297481,24.4770403834683,-7.44255185272593));
#9568=CARTESIAN_POINT('Ctrl Pts',(82.7114862915396,24.733670147315,-7.47959622538978));
#9569=CARTESIAN_POINT('Ctrl Pts',(83.3393622843697,24.7244378244931,-7.51664059805363));
#9570=CARTESIAN_POINT('Ctrl Pts',(83.8196958818033,24.4535682023601,-7.55368497071749));
#9571=CARTESIAN_POINT('Ctrl Pts',(84.300029479237,24.182698580227,-7.59072934338134));
#9572=CARTESIAN_POINT('Ctrl Pts',(84.6328206812744,23.6501916587828,-7.62777371604519));
#9573=CARTESIAN_POINT('Ctrl Pts',(84.6657776422957,23.0997331376905,-7.66481808870905));
#9574=CARTESIAN_POINT('Ctrl Pts',(84.6987346033171,22.5492746165983,-7.7018624613729));
#9575=CARTESIAN_POINT('Ctrl Pts',(84.4318573233225,21.9808644958579,-7.73890683403675));
#9576=CARTESIAN_POINT('Ctrl Pts',(83.9872741189408,21.6546184064601,-7.77595120670061));
#9577=CARTESIAN_POINT('Ctrl Pts',(83.5426909145591,21.3283723170624,-7.81299557936446));
#9578=CARTESIAN_POINT('Ctrl Pts',(82.9204017857903,21.2442902590072,-7.85003995202831));
#9579=CARTESIAN_POINT('Ctrl Pts',(82.4051784738551,21.4408498500478,-7.88708432469217));
#9580=CARTESIAN_POINT('Ctrl Pts',(81.8899551619199,21.6374094410885,-7.92412869735602));
#9581=CARTESIAN_POINT('Ctrl Pts',(81.4817976668182,22.1146106812249,-7.96117307001987));
#9582=CARTESIAN_POINT('Ctrl Pts',(81.3674868961021,22.6540768850889,-7.99821744268373));
#9583=CARTESIAN_POINT('Ctrl Pts',(81.3435588137885,22.7670005549285,-8.00597174958589));
#9584=CARTESIAN_POINT('Ctrl Pts',(81.3325061790855,22.8826524814131,-8.01372605648805));
#9585=CARTESIAN_POINT('Ctrl Pts',(81.3335754310806,22.9985070363431,-8.02148036339021));
#9586=CARTESIAN_POINT('Ctrl Pts',(81.3366057744099,22.9995801773856,-7.82851963660979));
#9587=CARTESIAN_POINT('Ctrl Pts',(81.3360371671033,22.7474696331785,-7.81172305369484));
#9588=CARTESIAN_POINT('Ctrl Pts',(81.3897674449501,22.4955891030212,-7.7949264707799));
#9589=CARTESIAN_POINT('Ctrl Pts',(81.4990408624314,22.2706965303371,-7.77812988786495));
#9590=CARTESIAN_POINT('Ctrl Pts',(81.7400401906833,21.774702534771,-7.7410855152011));
#9591=CARTESIAN_POINT('Ctrl Pts',(82.2512069777315,21.4099806987659,-7.70404114253724));
#9592=CARTESIAN_POINT('Ctrl Pts',(82.7986212516801,21.3434347775978,-7.66699676987339));
#9593=CARTESIAN_POINT('Ctrl Pts',(83.3460355256286,21.2768888564297,-7.62995239720953));
#9594=CARTESIAN_POINT('Ctrl Pts',(83.9296972864776,21.5085188500986,-7.59290802454568));
#9595=CARTESIAN_POINT('Ctrl Pts',(84.2825114071208,21.9323265833871,-7.55586365188183));
#9596=CARTESIAN_POINT('Ctrl Pts',(84.635325527764,22.3561343166757,-7.51881927921797));
#9597=CARTESIAN_POINT('Ctrl Pts',(84.7572920082014,22.972119789584,-7.48177490655412));
#9598=CARTESIAN_POINT('Ctrl Pts',(84.5925966245821,23.4983953920944,-7.44473053389027));
#9599=CARTESIAN_POINT('Ctrl Pts',(84.4279012409627,24.0246709946049,-7.40768616122641));
#9600=CARTESIAN_POINT('Ctrl Pts',(83.9765439932867,24.4612367267175,-7.37064178856256));
#9601=CARTESIAN_POINT('Ctrl Pts',(83.445074765178,24.608312585173,-7.33359741589871));
#9602=CARTESIAN_POINT('Ctrl Pts',(82.9136055370693,24.7553884436286,-7.29655304323486));
#9603=CARTESIAN_POINT('Ctrl Pts',(82.302024328528,24.6129744284271,-7.259508670571));
#9604=CARTESIAN_POINT('Ctrl Pts',(81.8902028870342,24.2462398670019,-7.22246429790715));
#9605=CARTESIAN_POINT('Ctrl Pts',(81.542076005189,23.9362264814174,-7.19114941080803));
#9606=CARTESIAN_POINT('Ctrl Pts',(81.3366955463558,23.4659157744314,-7.15983452370891));
#9607=CARTESIAN_POINT('Ctrl Pts',(81.3326822579993,22.9986976815004,-7.12851963660979));
#9608=CARTESIAN_POINT('Origin',(83.,23.,-12.));
#9609=CARTESIAN_POINT('',(81.3325224760112,23.0012132743929,-6.42851963660979));
#9610=CARTESIAN_POINT('',(81.3361556106367,23.000944168981,-6.62148036339021));
#9611=CARTESIAN_POINT('',(81.334,23.,-12.));
#9612=CARTESIAN_POINT('',(84.2690708798524,24.0793586530485,-6.));
#9613=CARTESIAN_POINT('Ctrl Pts',(81.3325224760112,23.0012132743929,-6.42851963660979));
#9614=CARTESIAN_POINT('Ctrl Pts',(81.336457103811,22.5283745880917,-6.39681287573142));
#9615=CARTESIAN_POINT('Ctrl Pts',(81.5476198272028,22.0525508339784,-6.36510611485305));
#9616=CARTESIAN_POINT('Ctrl Pts',(81.9034041940898,21.742267204439,-6.33339935397468));
#9617=CARTESIAN_POINT('Ctrl Pts',(82.3190823746991,21.379749492578,-6.29635498131082));
#9618=CARTESIAN_POINT('Ctrl Pts',(82.9321727728451,21.2431982563679,-6.25931060864697));
#9619=CARTESIAN_POINT('Ctrl Pts',(83.4620472172122,21.3961907172468,-6.22226623598311));
#9620=CARTESIAN_POINT('Ctrl Pts',(83.9919216615793,21.5491831781257,-6.18522186331926));
#9621=CARTESIAN_POINT('Ctrl Pts',(84.4385801521673,21.9917193360936,-6.14817749065541));
#9622=CARTESIAN_POINT('Ctrl Pts',(84.5975917113444,22.5187686702513,-6.11113311799156));
#9623=CARTESIAN_POINT('Ctrl Pts',(84.7566032705217,23.0458180044091,-6.0740887453277));
#9624=CARTESIAN_POINT('Ctrl Pts',(84.627967898288,23.6573805147568,-6.03704437266385));
#9625=CARTESIAN_POINT('Ctrl Pts',(84.2690708798524,24.0793586530485,-6.));
#9626=CARTESIAN_POINT('',(81.7285276007435,24.0812047294779,-6.));
#9627=CARTESIAN_POINT('Origin',(83.,23.,-6.));
#9628=CARTESIAN_POINT('Ctrl Pts',(81.7285261364169,24.0812058551231,-6.));
#9629=CARTESIAN_POINT('Ctrl Pts',(82.0793423217202,24.4926754274034,-6.03631814560908));
#9630=CARTESIAN_POINT('Ctrl Pts',(82.6492094921542,24.7187178987082,-6.07263629121814));
#9631=CARTESIAN_POINT('Ctrl Pts',(83.1865491604904,24.6581958582692,-6.10895443682721));
#9632=CARTESIAN_POINT('Ctrl Pts',(83.7346336121355,24.5964636034197,-6.14599880949106));
#9633=CARTESIAN_POINT('Ctrl Pts',(84.2488766988198,24.2365918173637,-6.18304318215492));
#9634=CARTESIAN_POINT('Ctrl Pts',(84.4942852948547,23.742845889402,-6.22008755481878));
#9635=CARTESIAN_POINT('Ctrl Pts',(84.7396938908897,23.2490999614404,-6.25713192748263));
#9636=CARTESIAN_POINT('Ctrl Pts',(84.7162679962753,22.6214798915731,-6.29417630014648));
#9637=CARTESIAN_POINT('Ctrl Pts',(84.4345602009582,22.1474061483613,-6.33122067281033));
#9638=CARTESIAN_POINT('Ctrl Pts',(84.1528524056412,21.6733324051495,-6.36826504547418));
#9639=CARTESIAN_POINT('Ctrl Pts',(83.6128627096214,21.3528049885932,-6.40530941813804));
#9640=CARTESIAN_POINT('Ctrl Pts',(83.0617850229002,21.3323987424867,-6.44235379080189));
#9641=CARTESIAN_POINT('Ctrl Pts',(82.5107073361791,21.3119924963801,-6.47939816346575));
#9642=CARTESIAN_POINT('Ctrl Pts',(81.9485416587566,21.5917074207234,-6.5164425361296));
#9643=CARTESIAN_POINT('Ctrl Pts',(81.6325039520559,22.0435930082728,-6.55348690879345));
#9644=CARTESIAN_POINT('Ctrl Pts',(81.4391457897928,22.3200656091972,-6.57615139365904));
#9645=CARTESIAN_POINT('Ctrl Pts',(81.3379191370965,22.6609857536405,-6.59881587852463));
#9646=CARTESIAN_POINT('Ctrl Pts',(81.3361556106367,23.000944168981,-6.62148036339021));
#9647=CARTESIAN_POINT('Origin',(83.,23.,-4.45407471946233));
#9648=CARTESIAN_POINT('',(80.9445918561381,23.001823176295,-16.6459252805377));
#9649=CARTESIAN_POINT('',(80.9470731721499,22.9984940384348,-16.7040747194623));
#9650=CARTESIAN_POINT('',(80.94525,23.0000000000001,-4.45407471946233));
#9651=CARTESIAN_POINT('',(84.8174278887595,23.9586205879593,-17.));
#9652=CARTESIAN_POINT('Ctrl Pts',(80.9470731721499,22.9984940384348,-16.7040747194623));
#9653=CARTESIAN_POINT('Ctrl Pts',(80.9500636069218,23.452419291778,-16.7286277343139));
#9654=CARTESIAN_POINT('Ctrl Pts',(81.3216921078483,24.5959829414065,-16.7902251218292));
#9655=CARTESIAN_POINT('Ctrl Pts',(83.2159905896636,25.4179577199457,-16.8888668820084));
#9656=CARTESIAN_POINT('Ctrl Pts',(84.4986774253636,24.5629326473987,-16.9629556273361));
#9657=CARTESIAN_POINT('Ctrl Pts',(84.8174278887595,23.9586205879593,-17.));
#9658=CARTESIAN_POINT('',(85.0570979162306,22.9245442276038,-17.));
#9659=CARTESIAN_POINT('Origin',(83.,23.,-17.));
#9660=CARTESIAN_POINT('Ctrl Pts',(80.9445918561382,23.001823176295,-16.6459252805377));
#9661=CARTESIAN_POINT('Ctrl Pts',(80.9432972802338,23.1421867341789,-16.6535432960883));
#9662=CARTESIAN_POINT('Ctrl Pts',(81.0204256104681,23.9636912996603,-16.6982056843029));
#9663=CARTESIAN_POINT('Ctrl Pts',(82.12637451265,25.2659591550417,-16.7799124451812));
#9664=CARTESIAN_POINT('Ctrl Pts',(84.4138508336827,24.965114478167,-16.890319336118));
#9665=CARTESIAN_POINT('Ctrl Pts',(85.0806816951007,23.591021626778,-16.9636818543909));
#9666=CARTESIAN_POINT('Ctrl Pts',(85.0571001857713,22.9245440319506,-17.));
#9667=CARTESIAN_POINT('Origin',(83.,23.,-4.45407471946233));
#9668=CARTESIAN_POINT('',(80.9485828438711,22.9999504095115,-15.9459252805377));
#9669=CARTESIAN_POINT('',(80.941985868441,22.999516909691,-16.0040747194623));
#9670=CARTESIAN_POINT('',(80.94525,23.0000000000001,-4.45407471946233));
#9671=CARTESIAN_POINT('Ctrl Pts',(80.941985868441,22.999516909691,-16.0040747194623));
#9672=CARTESIAN_POINT('Ctrl Pts',(80.9440549059599,23.6536076635307,-16.0396948316641));
#9673=CARTESIAN_POINT('Ctrl Pts',(81.6350686818089,24.9917162152022,-16.1123593165296));
#9674=CARTESIAN_POINT('Ctrl Pts',(83.9141747198462,25.2499873352066,-16.2220681740591));
#9675=CARTESIAN_POINT('Ctrl Pts',(85.3860300953815,23.4524069852193,-16.3332012920506));
#9676=CARTESIAN_POINT('Ctrl Pts',(84.6743954809949,21.240621211679,-16.4443344100422));
#9677=CARTESIAN_POINT('Ctrl Pts',(82.4296924778299,20.6393768340819,-16.5554675280338));
#9678=CARTESIAN_POINT('Ctrl Pts',(81.0884934760466,21.8537197383225,-16.6420476311738));
#9679=CARTESIAN_POINT('Ctrl Pts',(80.9455517870582,22.767559353067,-16.69158336165));
#9680=CARTESIAN_POINT('Ctrl Pts',(80.9470731721499,22.9984940384348,-16.7040747194623));
#9681=CARTESIAN_POINT('Ctrl Pts',(80.9485828438712,22.9999504095115,-15.9459252805377));
#9682=CARTESIAN_POINT('Ctrl Pts',(80.9486568620999,23.34590005549,-15.9646103934386));
#9683=CARTESIAN_POINT('Ctrl Pts',(81.1957456616406,24.3778157149169,-16.0203398790033));
#9684=CARTESIAN_POINT('Ctrl Pts',(82.8298598776186,25.4226489294061,-16.1131137372319));
#9685=CARTESIAN_POINT('Ctrl Pts',(84.9430514056717,24.4569400344173,-16.2242468552234));
#9686=CARTESIAN_POINT('Ctrl Pts',(85.2779271552008,22.1577886838534,-16.335379973215));
#9687=CARTESIAN_POINT('Ctrl Pts',(83.5278718544653,20.6294494978248,-16.4465130912065));
#9688=CARTESIAN_POINT('Ctrl Pts',(81.4479222208321,21.2267962234199,-16.5500281936475));
#9689=CARTESIAN_POINT('Ctrl Pts',(80.9495924567037,22.4596362835927,-16.6164989234245));
#9690=CARTESIAN_POINT('Ctrl Pts',(80.9445918561382,23.001823176295,-16.6459252805377));
#9691=CARTESIAN_POINT('Origin',(83.,23.,-4.45407471946233));
#9692=CARTESIAN_POINT('',(80.9444684385758,22.9981936684133,-15.2459252805377));
#9693=CARTESIAN_POINT('',(80.9457759848993,23.001865484283,-15.3040747194623));
#9694=CARTESIAN_POINT('',(80.94525,23.0000000000001,-4.45407471946233));
#9695=CARTESIAN_POINT('Ctrl Pts',(80.9457759848993,23.001865484283,-15.3040747194623));
#9696=CARTESIAN_POINT('Ctrl Pts',(80.9441908674823,23.179786033038,-15.3137175563504));
#9697=CARTESIAN_POINT('Ctrl Pts',(81.0468089400269,24.039414645723,-15.3604047659024));
#9698=CARTESIAN_POINT('Ctrl Pts',(82.2507940260338,25.3101655411,-15.4441363481181));
#9699=CARTESIAN_POINT('Ctrl Pts',(84.5344926196224,24.8824203570357,-15.5552694661097));
#9700=CARTESIAN_POINT('Ctrl Pts',(85.4137607912389,22.7318111240602,-15.6664025841013));
#9701=CARTESIAN_POINT('Ctrl Pts',(84.0838648276161,20.8266566062216,-15.7775357020929));
#9702=CARTESIAN_POINT('Ctrl Pts',(81.7619636485858,20.9106360913409,-15.8886688200844));
#9703=CARTESIAN_POINT('Ctrl Pts',(80.9542066368151,22.2670451103755,-15.9641818258742));
#9704=CARTESIAN_POINT('Ctrl Pts',(80.9419031385406,22.9733632694651,-16.0026504590002));
#9705=CARTESIAN_POINT('Ctrl Pts',(80.941985868441,22.999516909691,-16.0040747194623));
#9706=CARTESIAN_POINT('Ctrl Pts',(80.9444684385758,22.9981936684133,-15.2459252805377));
#9707=CARTESIAN_POINT('Ctrl Pts',(80.9494988573722,23.5462600854287,-15.2756774907888));
#9708=CARTESIAN_POINT('Ctrl Pts',(81.4568946603439,24.7849447934067,-15.3424740737037));
#9709=CARTESIAN_POINT('Ctrl Pts',(83.5486977451864,25.3658199574776,-15.4463150292825));
#9710=CARTESIAN_POINT('Ctrl Pts',(85.2852062155397,23.822195101775,-15.5574481472741));
#9711=CARTESIAN_POINT('Ctrl Pts',(84.9302046695978,21.5260650294792,-15.6685812652657));
#9712=CARTESIAN_POINT('Ctrl Pts',(82.8086025275965,20.5789380526202,-15.7797143832572));
#9713=CARTESIAN_POINT('Ctrl Pts',(81.1894352243962,21.6343485525749,-15.8721623883479));
#9714=CARTESIAN_POINT('Ctrl Pts',(80.9485101164599,22.6600338433596,-15.9275660207747));
#9715=CARTESIAN_POINT('Ctrl Pts',(80.9485828438712,22.9999504095115,-15.9459252805377));
#9716=CARTESIAN_POINT('Origin',(83.,23.,-4.45407471946233));
#9717=CARTESIAN_POINT('',(80.9427069405049,23.0011828703653,-14.5459252805377));
#9718=CARTESIAN_POINT('',(80.9483910840592,22.9993486074027,-14.6040747194623));
#9719=CARTESIAN_POINT('',(80.94525,23.0000000000001,-4.45407471946233));
#9720=CARTESIAN_POINT('Ctrl Pts',(80.9483910840592,22.9993486074027,-14.6040747194623));
#9721=CARTESIAN_POINT('Ctrl Pts',(80.9494811123425,23.3826976046307,-14.6247846537006));
#9722=CARTESIAN_POINT('Ctrl Pts',(81.2366608737661,24.4532689341001,-14.6825389606028));
#9723=CARTESIAN_POINT('Ctrl Pts',(82.9621345872503,25.4283202829728,-14.7773376401688));
#9724=CARTESIAN_POINT('Ctrl Pts',(85.0195747495924,24.3488851074018,-14.8884707581604));
#9725=CARTESIAN_POINT('Ctrl Pts',(85.2286205736113,22.0348972082601,-14.9996038761519));
#9726=CARTESIAN_POINT('Ctrl Pts',(83.3979452064162,20.6042093336492,-15.1107369941435));
#9727=CARTESIAN_POINT('Ctrl Pts',(81.3935016039341,21.3001230071733,-15.2122272752469));
#9728=CARTESIAN_POINT('Ctrl Pts',(80.9502803286018,22.4962781412084,-15.2766731836866));
#9729=CARTESIAN_POINT('Ctrl Pts',(80.9457759848993,23.001865484283,-15.3040747194623));
#9730=CARTESIAN_POINT('Ctrl Pts',(80.9427069405049,23.0011828703653,-14.5459252805377));
#9731=CARTESIAN_POINT('Ctrl Pts',(80.9422307466888,23.0705663228386,-14.5497002154751));
#9732=CARTESIAN_POINT('Ctrl Pts',(80.9768964145428,23.8203453482233,-14.5905195230765));
#9733=CARTESIAN_POINT('Ctrl Pts',(81.8966144503262,25.1634956547744,-14.6683832033416));
#9734=CARTESIAN_POINT('Ctrl Pts',(84.2191696572937,25.1004281633947,-14.7795163213332));
#9735=CARTESIAN_POINT('Ctrl Pts',(85.4258928026212,23.1149661440179,-14.8906494393247));
#9736=CARTESIAN_POINT('Ctrl Pts',(84.4123433832198,21.0242825862308,-15.0017825573163));
#9737=CARTESIAN_POINT('Ctrl Pts',(82.1061616893797,20.7418533657775,-15.1129156753078));
#9738=CARTESIAN_POINT('Ctrl Pts',(81.0164470233792,22.0484774837239,-15.1942965830483));
#9739=CARTESIAN_POINT('Ctrl Pts',(80.9432355005669,22.8638645112809,-15.2386331181249));
#9740=CARTESIAN_POINT('Ctrl Pts',(80.9444684385758,22.9981936684133,-15.2459252805377));
#9741=CARTESIAN_POINT('Origin',(83.,23.,-4.45407471946233));
#9742=CARTESIAN_POINT('',(80.9480449766009,23.0010551249669,-13.8459252805377));
#9743=CARTESIAN_POINT('',(80.9433898278768,22.9984792505039,-13.9040747194623));
#9744=CARTESIAN_POINT('',(80.94525,23.0000000000001,-4.45407471946233));
#9745=CARTESIAN_POINT('Ctrl Pts',(80.9433898278768,22.9984792505039,-13.9040747194623));
#9746=CARTESIAN_POINT('Ctrl Pts',(80.948232962241,23.5830502245177,-13.9358517510509));
#9747=CARTESIAN_POINT('Ctrl Pts',(81.5151171939793,24.8573002990708,-14.0046731553032));
#9748=CARTESIAN_POINT('Ctrl Pts',(83.6768129281338,25.3324016450226,-14.1105389322195));
#9749=CARTESIAN_POINT('Ctrl Pts',(85.3266177853476,23.6964358225195,-14.221672050211));
#9750=CARTESIAN_POINT('Ctrl Pts',(84.8470104700268,21.423064524091,-14.3328051682026));
#9751=CARTESIAN_POINT('Ctrl Pts',(82.676946476112,20.5929666402091,-14.4439382861941));
#9752=CARTESIAN_POINT('Ctrl Pts',(81.1518515427802,21.7100345132185,-14.5343614699474));
#9753=CARTESIAN_POINT('Ctrl Pts',(80.9475313517361,22.6969917520569,-14.5877402810368));
#9754=CARTESIAN_POINT('Ctrl Pts',(80.9483910840592,22.9993486074027,-14.6040747194623));
#9755=CARTESIAN_POINT('Ctrl Pts',(80.9480449766009,23.001055124967,-13.8459252805377));
#9756=CARTESIAN_POINT('Ctrl Pts',(80.9467671657193,23.2756711098727,-13.8607673128254));
#9757=CARTESIAN_POINT('Ctrl Pts',(81.1259274853824,24.2341048917329,-13.9126537177769));
#9758=CARTESIAN_POINT('Ctrl Pts',(82.5805008911621,25.3921107031273,-14.0015844953923));
#9759=CARTESIAN_POINT('Ctrl Pts',(84.7821632663096,24.6498688464973,-14.1127176133838));
#9760=CARTESIAN_POINT('Ctrl Pts',(85.3527196747847,22.397602083335,-14.2238507313754));
#9761=CARTESIAN_POINT('Ctrl Pts',(83.7699744349188,20.6966736036812,-14.3349838493669));
#9762=CARTESIAN_POINT('Ctrl Pts',(81.5602178798653,21.0900095959384,-14.442342032421));
#9763=CARTESIAN_POINT('Ctrl Pts',(80.9469037546942,22.3896892977476,-14.5126558428113));
#9764=CARTESIAN_POINT('Ctrl Pts',(80.9427069405049,23.0011828703653,-14.5459252805377));
#9765=CARTESIAN_POINT('Origin',(83.,23.,-4.45407471946233));
#9766=CARTESIAN_POINT('',(80.9465558937026,22.998246285774,-13.1459252805377));
#9767=CARTESIAN_POINT('',(80.9436610901855,23.0016161418076,-13.2040747194623));
#9768=CARTESIAN_POINT('',(80.94525,23.0000000000001,-4.45407471946233));
#9769=CARTESIAN_POINT('Ctrl Pts',(80.9436610901855,23.0016161418076,-13.2040747194623));
#9770=CARTESIAN_POINT('Ctrl Pts',(80.9427399464891,23.1083452056402,-13.2098744757372));
#9771=CARTESIAN_POINT('Ctrl Pts',(80.9988245257335,23.895806936048,-13.252718604676));
#9772=CARTESIAN_POINT('Ctrl Pts',(82.0161587277924,25.2204120168147,-13.3326071062785));
#9773=CARTESIAN_POINT('Ctrl Pts',(84.3318254372397,25.0308653766405,-13.4437402242701));
#9774=CARTESIAN_POINT('Ctrl Pts',(85.4285530863916,22.9825908096803,-13.5548733422617));
#9775=CARTESIAN_POINT('Ctrl Pts',(84.3025733639503,20.9502498189244,-13.6660064602532));
#9776=CARTESIAN_POINT('Ctrl Pts',(81.9844272300528,20.7939208712606,-13.7771395782448));
#9777=CARTESIAN_POINT('Ctrl Pts',(80.992840331298,22.1240505870937,-13.8564956646478));
#9778=CARTESIAN_POINT('Ctrl Pts',(80.9425870329241,22.9015811278996,-13.898807378387));
#9779=CARTESIAN_POINT('Ctrl Pts',(80.9433898278768,22.9984792505039,-13.9040747194623));
#9780=CARTESIAN_POINT('Ctrl Pts',(80.9465558937026,22.998246285774,-13.1459252805377));
#9781=CARTESIAN_POINT('Ctrl Pts',(80.950443637898,23.4767580065597,-13.1718344101756));
#9782=CARTESIAN_POINT('Ctrl Pts',(81.3555437322658,24.6453701880592,-13.2347879124773));
#9783=CARTESIAN_POINT('Ctrl Pts',(83.3013691324087,25.409844344426,-13.3347857874429));
#9784=CARTESIAN_POINT('Ctrl Pts',(85.1880466324256,24.0538619704037,-13.4459189054344));
#9785=CARTESIAN_POINT('Ctrl Pts',(85.0721377337693,21.7333436414648,-13.557052023426));
#9786=CARTESIAN_POINT('Ctrl Pts',(83.0597268226234,20.5721190669662,-13.6681851414176));
#9787=CARTESIAN_POINT('Ctrl Pts',(81.2687132736902,21.4913058617477,-13.7644762271215));
#9788=CARTESIAN_POINT('Ctrl Pts',(80.94995646632,22.5902544036478,-13.8237229401615));
#9789=CARTESIAN_POINT('Ctrl Pts',(80.9480449766009,23.001055124967,-13.8459252805377));
#9790=CARTESIAN_POINT('Origin',(83.,23.,-4.45407471946233));
#9791=CARTESIAN_POINT('',(80.9418454804923,22.9999766228626,-12.4459252805377));
#9792=CARTESIAN_POINT('',(80.9484733990566,23.0004971809245,-12.5040747194623));
#9793=CARTESIAN_POINT('',(80.94525,23.0000000000001,-4.45407471946233));
#9794=CARTESIAN_POINT('Ctrl Pts',(80.9484733990566,23.0004971809245,-12.5040747194623));
#9795=CARTESIAN_POINT('Ctrl Pts',(80.9477973499854,23.3127405278041,-12.5209415730874));
#9796=CARTESIAN_POINT('Ctrl Pts',(81.1614616883935,24.3098806979921,-12.5748527993764));
#9797=CARTESIAN_POINT('Ctrl Pts',(82.7114877530095,25.4114173957764,-12.6658083983292));
#9798=CARTESIAN_POINT('Ctrl Pts',(84.8694281534639,24.5502940212596,-12.7769415163208));
#9799=CARTESIAN_POINT('Ctrl Pts',(85.3163943278932,22.2702805395079,-12.8880746343123));
#9800=CARTESIAN_POINT('Ctrl Pts',(83.6433052410424,20.6581350294767,-12.9992077523039));
#9801=CARTESIAN_POINT('Ctrl Pts',(81.4994790128079,21.1616334099512,-13.1045411140205));
#9802=CARTESIAN_POINT('Ctrl Pts',(80.9486235024093,22.4266422120513,-13.1728301030734));
#9803=CARTESIAN_POINT('Ctrl Pts',(80.9436610901855,23.0016161418076,-13.2040747194623));
#9804=CARTESIAN_POINT('Ctrl Pts',(80.941845609139,22.999976623746,-12.4459252805377));
#9805=CARTESIAN_POINT('Ctrl Pts',(80.9419597659312,23.6788458613235,-12.4829015075258));
#9806=CARTESIAN_POINT('Ctrl Pts',(81.6804454174154,25.0380482591789,-12.5569221071778));
#9807=CARTESIAN_POINT('Ctrl Pts',(83.9956695619749,25.2151332333942,-12.6679870794935));
#9808=CARTESIAN_POINT('Ctrl Pts',(85.4010382767464,23.364949738908,-12.7791201974851));
#9809=CARTESIAN_POINT('Ctrl Pts',(84.6088822566941,21.1807498790914,-12.8902533154767));
#9810=CARTESIAN_POINT('Ctrl Pts',(82.3442138703267,20.6615993349174,-13.0013864334682));
#9811=CARTESIAN_POINT('Ctrl Pts',(81.0677939508996,21.9047210022768,-13.0866104218219));
#9812=CARTESIAN_POINT('Ctrl Pts',(80.9448850164079,22.7925911990848,-13.1347900375117));
#9813=CARTESIAN_POINT('Ctrl Pts',(80.9465558937026,22.998246285774,-13.1459252805377));
#9814=CARTESIAN_POINT('Origin',(83.,23.,-4.45407471946233));
#9815=CARTESIAN_POINT('',(80.946487742054,23.0017684726493,-11.7459252805377));
#9816=CARTESIAN_POINT('',(80.9454838921393,22.9981221128236,-11.8040747194623));
#9817=CARTESIAN_POINT('',(80.94525,23.0000000000001,-4.45407471946233));
#9818=CARTESIAN_POINT('Ctrl Pts',(80.9454838921393,22.9981221128236,-11.8040747194623));
#9819=CARTESIAN_POINT('Ctrl Pts',(80.9501624736055,23.5133464089528,-11.8320086704376));
#9820=CARTESIAN_POINT('Ctrl Pts',(81.4074703003843,24.7192340376815,-11.8969869940768));
#9821=CARTESIAN_POINT('Ctrl Pts',(83.4322511648908,25.3898393468531,-11.9990096903799));
#9822=CARTESIAN_POINT('Ctrl Pts',(85.2422276109297,23.9330533286481,-12.1101428083714));
#9823=CARTESIAN_POINT('Ctrl Pts',(85.000029094227,21.6223001794432,-12.221275926363));
#9824=CARTESIAN_POINT('Ctrl Pts',(82.9273252301097,20.5724721317484,-12.3324090443545));
#9825=CARTESIAN_POINT('Ctrl Pts',(81.2256187435467,21.5665457480708,-12.426675308721));
#9826=CARTESIAN_POINT('Ctrl Pts',(80.9492821446181,22.626965980831,-12.4838972004236));
#9827=CARTESIAN_POINT('Ctrl Pts',(80.9484733990566,23.0004971809245,-12.5040747194623));
#9828=CARTESIAN_POINT('Ctrl Pts',(80.946487742054,23.0017684726493,-11.7459252805377));
#9829=CARTESIAN_POINT('Ctrl Pts',(80.9448193888947,23.2048893572511,-11.7569242322121));
#9830=CARTESIAN_POINT('Ctrl Pts',(81.0658212075453,24.0901758494269,-11.8049675565505));
#9831=CARTESIAN_POINT('Ctrl Pts',(82.3356362705467,25.3359781577142,-11.8900552535526));
#9832=CARTESIAN_POINT('Ctrl Pts',(84.6021947068076,24.825142525889,-12.0011883715442));
#9833=CARTESIAN_POINT('Ctrl Pts',(85.4023614856292,22.6438646174604,-12.1123214895358));
#9834=CARTESIAN_POINT('Ctrl Pts',(84.0037924767762,20.7885358284841,-12.2234546075273));
#9835=CARTESIAN_POINT('Ctrl Pts',(81.6865130842908,20.9572260916608,-12.3345877255189));
#9836=CARTESIAN_POINT('Ctrl Pts',(80.9424129889364,22.3173541979826,-12.4087446165223));
#9837=CARTESIAN_POINT('Ctrl Pts',(80.9418453987527,22.9987254954749,-12.4458571348619));
#9838=CARTESIAN_POINT('Ctrl Pts',(80.941845609139,22.999976623746,-12.4459252805377));
#9839=CARTESIAN_POINT('Origin',(83.,23.,-4.45407471946233));
#9840=CARTESIAN_POINT('',(80.9480833902501,22.9989795845752,-11.0459252805377));
#9841=CARTESIAN_POINT('',(80.942099557822,23.0006544392887,-11.1040747194623));
#9842=CARTESIAN_POINT('',(80.94525,23.0000000000001,-4.45407471946233));
#9843=CARTESIAN_POINT('Ctrl Pts',(80.942099557822,23.0006544392887,-11.1040747194623));
#9844=CARTESIAN_POINT('Ctrl Pts',(80.941949761973,23.0365901265997,-11.106031395124));
#9845=CARTESIAN_POINT('Ctrl Pts',(80.9590874886889,23.7527252524841,-11.1450324434495));
#9846=CARTESIAN_POINT('Ctrl Pts',(81.7920500466204,25.1069005869871,-11.2210778644389));
#9847=CARTESIAN_POINT('Ctrl Pts',(84.1149085920925,25.1575801270393,-11.3322109824305));
#9848=CARTESIAN_POINT('Ctrl Pts',(85.4173589117072,23.2335574132988,-11.4433441004221));
#9849=CARTESIAN_POINT('Ctrl Pts',(84.5073472090078,21.0957737621771,-11.5544772184136));
#9850=CARTESIAN_POINT('Ctrl Pts',(82.2177520120164,20.7008129135252,-11.6656103364052));
#9851=CARTESIAN_POINT('Ctrl Pts',(81.0396472413493,21.980504676805,-11.7488095034214));
#9852=CARTESIAN_POINT('Ctrl Pts',(80.9439580123917,22.8300860692986,-11.7949642977738));
#9853=CARTESIAN_POINT('Ctrl Pts',(80.9454838921393,22.9981221128236,-11.8040747194623));
#9854=CARTESIAN_POINT('Ctrl Pts',(80.9480833902501,22.9989795845752,-11.0459252805377));
#9855=CARTESIAN_POINT('Ctrl Pts',(80.9499186191076,23.4072776930713,-11.0679913295624));
#9856=CARTESIAN_POINT('Ctrl Pts',(81.2657181967231,24.5036404128733,-11.1271017512509));
#9857=CARTESIAN_POINT('Ctrl Pts',(83.0508160082765,25.4280837818398,-11.2232565456033));
#9858=CARTESIAN_POINT('Ctrl Pts',(85.0674751034236,24.2742526496163,-11.3343896635948));
#9859=CARTESIAN_POINT('Ctrl Pts',(85.1918996088904,21.9541753383684,-11.4455227815864));
#9860=CARTESIAN_POINT('Ctrl Pts',(83.3102113199728,20.5912779207033,-11.5566558995779));
#9861=CARTESIAN_POINT('Ctrl Pts',(81.3589375218264,21.3496378721918,-11.6567900658951));
#9862=CARTESIAN_POINT('Ctrl Pts',(80.9504383876862,22.5207800014051,-11.7198798595483));
#9863=CARTESIAN_POINT('Ctrl Pts',(80.946487742054,23.0017684726493,-11.7459252805377));
#9864=CARTESIAN_POINT('Origin',(83.,23.,-4.45407471946233));
#9865=CARTESIAN_POINT('',(80.9427635247896,22.9987822671278,-10.3459252805377));
#9866=CARTESIAN_POINT('',(80.9474130033736,23.0014635246622,-10.4040747194623));
#9867=CARTESIAN_POINT('',(80.94525,23.0000000000001,-4.45407471946233));
#9868=CARTESIAN_POINT('Ctrl Pts',(80.9474130033736,23.0014635246621,-10.4040747194623));
#9869=CARTESIAN_POINT('Ctrl Pts',(80.9458279183746,23.2422509457676,-10.4170984924742));
#9870=CARTESIAN_POINT('Ctrl Pts',(81.0963187654959,24.1660078235155,-10.46716663815));
#9871=CARTESIAN_POINT('Ctrl Pts',(82.4639279501368,25.3687127159435,-10.5542791564896));
#9872=CARTESIAN_POINT('Ctrl Pts',(84.6992789742144,24.7351150224436,-10.6654122744811));
#9873=CARTESIAN_POINT('Ctrl Pts',(85.3793829981224,22.5134717669416,-10.7765453924727));
#9874=CARTESIAN_POINT('Ctrl Pts',(83.8817820505465,20.7371182998993,-10.8876785104642));
#9875=CARTESIAN_POINT('Ctrl Pts',(81.617716369494,21.0266541288133,-10.9968549527941));
#9876=CARTESIAN_POINT('Ctrl Pts',(80.9447857420797,22.3562448763623,-11.0689870224602));
#9877=CARTESIAN_POINT('Ctrl Pts',(80.942099557822,23.0006544392887,-11.1040747194623));
#9878=CARTESIAN_POINT('Ctrl Pts',(80.9427635247896,22.9987822671278,-10.3459252805377));
#9879=CARTESIAN_POINT('Ctrl Pts',(80.9470399691646,23.6078148575591,-10.3790584269126));
#9880=CARTESIAN_POINT('Ctrl Pts',(81.5560212788413,24.9052031204881,-10.4492359459513));
#9881=CARTESIAN_POINT('Ctrl Pts',(83.7615159569619,25.3061367187622,-10.5564578376539));
#9882=CARTESIAN_POINT('Ctrl Pts',(85.3504930077305,23.6110284272776,-10.6675909556455));
#9883=CARTESIAN_POINT('Ctrl Pts',(84.7882063433206,21.3566828693041,-10.778724073637));
#9884=CARTESIAN_POINT('Ctrl Pts',(82.5892828503881,20.6063658296754,-10.8898571916286));
#9885=CARTESIAN_POINT('Ctrl Pts',(81.1282336040668,21.7607920195001,-10.9789242605955));
#9886=CARTESIAN_POINT('Ctrl Pts',(80.9468376460868,22.7218288720269,-11.0309469568985));
#9887=CARTESIAN_POINT('Ctrl Pts',(80.9480833902501,22.9989795845752,-11.0459252805377));
#9888=CARTESIAN_POINT('Origin',(83.,23.,-4.45407471946233));
#9889=CARTESIAN_POINT('',(80.944392795472,23.0017938245641,-9.64592528053768));
#9890=CARTESIAN_POINT('',(80.9473844340938,22.9985230105256,-9.70407471946232));
#9891=CARTESIAN_POINT('',(80.94525,23.0000000000001,-4.45407471946233));
#9892=CARTESIAN_POINT('Ctrl Pts',(80.9473844340938,22.9985230105256,-9.70407471946232));
#9893=CARTESIAN_POINT('Ctrl Pts',(80.9503460891386,23.4439066603514,-9.72816558982444));
#9894=CARTESIAN_POINT('Ctrl Pts',(81.3116442355096,24.5785301187141,-9.7893008328504));
#9895=CARTESIAN_POINT('Ctrl Pts',(83.1830643805896,25.4217061353262,-9.88748044854022));
#9896=CARTESIAN_POINT('Ctrl Pts',(85.1338459461496,24.1596873076041,-9.99861356653177));
#9897=CARTESIAN_POINT('Ctrl Pts',(85.1316477144354,21.8362770111152,-10.1097466845233));
#9898=CARTESIAN_POINT('Ctrl Pts',(83.1784815936336,20.5779517977441,-10.2208798025149));
#9899=CARTESIAN_POINT('Ctrl Pts',(81.3099985927049,21.4240614634891,-10.3189891474946));
#9900=CARTESIAN_POINT('Ctrl Pts',(80.9503364797073,22.5573634748289,-10.3800541198104));
#9901=CARTESIAN_POINT('Ctrl Pts',(80.9474130033736,23.0014635246621,-10.4040747194623));
#9902=CARTESIAN_POINT('Ctrl Pts',(80.944392795472,23.0017938245641,-9.64592528053768));
#9903=CARTESIAN_POINT('Ctrl Pts',(80.9431863548551,23.1335998594481,-9.65308115159894));
#9904=CARTESIAN_POINT('Ctrl Pts',(81.0147851841557,23.9464313285286,-9.69728139532405));
#9905=CARTESIAN_POINT('Ctrl Pts',(82.0978802396299,25.2548510053398,-9.778526011713));
#9906=CARTESIAN_POINT('Ctrl Pts',(84.4050829104209,24.9808874610066,-9.88965912970457));
#9907=CARTESIAN_POINT('Ctrl Pts',(85.4262983980702,22.8939377453899,-10.0007922476961));
#9908=CARTESIAN_POINT('Ctrl Pts',(84.2268700936312,20.9040603797618,-10.1119253656877));
#9909=CARTESIAN_POINT('Ctrl Pts',(81.9045619903646,20.8324694499553,-10.2230584836792));
#9910=CARTESIAN_POINT('Ctrl Pts',(80.9783022594501,22.1745804170201,-10.3010584552959));
#9911=CARTESIAN_POINT('Ctrl Pts',(80.9422587088125,22.9268885733755,-10.3420140542487));
#9912=CARTESIAN_POINT('Ctrl Pts',(80.9427635247896,22.9987822671278,-10.3459252805377));
#9913=CARTESIAN_POINT('Origin',(83.,23.,-4.45407471946233));
#9914=CARTESIAN_POINT('',(80.9485808590134,23.0000908847554,-8.94592528053768));
#9915=CARTESIAN_POINT('',(80.9420824460358,22.9993679634637,-9.00407471946233));
#9916=CARTESIAN_POINT('',(80.94525,23.0000000000001,-4.45407471946233));
#9917=CARTESIAN_POINT('Ctrl Pts',(80.9420824460358,22.9993679634637,-9.00407471946233));
#9918=CARTESIAN_POINT('Ctrl Pts',(80.9446923112335,23.6450537804481,-9.03923268717465));
#9919=CARTESIAN_POINT('Ctrl Pts',(81.6199952950891,24.9757743563403,-9.11143502755083));
#9920=CARTESIAN_POINT('Ctrl Pts',(83.8860623965075,25.2612091019686,-9.22068174059087));
#9921=CARTESIAN_POINT('Ctrl Pts',(85.3802993685163,23.4820249885188,-9.33181485858242));
#9922=CARTESIAN_POINT('Ctrl Pts',(84.6959926707885,21.2616726332633,-9.44294797657398));
#9923=CARTESIAN_POINT('Ctrl Pts',(82.4594467271343,20.632305903941,-9.55408109456555));
#9924=CARTESIAN_POINT('Ctrl Pts',(81.0952171682793,21.8366242266362,-9.64112334219499));
#9925=CARTESIAN_POINT('Ctrl Pts',(80.9457919716852,22.7590431558563,-9.69112121716058));
#9926=CARTESIAN_POINT('Ctrl Pts',(80.9473844340938,22.9985230105256,-9.70407471946232));
#9927=CARTESIAN_POINT('Ctrl Pts',(80.9485808590134,23.0000908847555,-8.94592528053767));
#9928=CARTESIAN_POINT('Ctrl Pts',(80.9484477321286,23.3374830514234,-8.96414824894915));
#9929=CARTESIAN_POINT('Ctrl Pts',(81.1868156697076,24.3605622630378,-9.01941559002447));
#9930=CARTESIAN_POINT('Ctrl Pts',(82.7997191606577,25.4203430963022,-9.11172730376366));
#9931=CARTESIAN_POINT('Ctrl Pts',(84.9247819088485,24.4810090214786,-9.22286042175521));
#9932=CARTESIAN_POINT('Ctrl Pts',(85.2882084953573,22.1861971982837,-9.33399353974677));
#9933=CARTESIAN_POINT('Ctrl Pts',(83.5573766039194,20.6362097301691,-9.44512665773833));
#9934=CARTESIAN_POINT('Ctrl Pts',(81.4607076296431,21.2101562866457,-9.54910390466863));
#9935=CARTESIAN_POINT('Ctrl Pts',(80.9494318329284,22.4512689686606,-9.61603677893508));
#9936=CARTESIAN_POINT('Ctrl Pts',(80.944392795472,23.0017938245641,-9.64592528053768));
#9937=CARTESIAN_POINT('Origin',(83.,23.,-4.45407471946233));
#9938=CARTESIAN_POINT('',(80.944726360752,22.998158663221,-8.24592528053768));
#9939=CARTESIAN_POINT('',(80.9455227171961,23.0018771067991,-8.30407471946232));
#9940=CARTESIAN_POINT('',(80.94525,23.0000000000001,-4.45407471946233));
#9941=CARTESIAN_POINT('Ctrl Pts',(80.9455227171961,23.0018771067991,-8.30407471946232));
#9942=CARTESIAN_POINT('Ctrl Pts',(80.9439882359492,23.1712174130647,-8.31325541186101));
#9943=CARTESIAN_POINT('Ctrl Pts',(81.0405828044266,24.0221240109118,-8.35948047692355));
#9944=CARTESIAN_POINT('Ctrl Pts',(82.2221040357635,25.3006631740422,-8.44274991464995));
#9945=CARTESIAN_POINT('Ctrl Pts',(84.5109477713164,24.9013705599747,-8.55388303264151));
#9946=CARTESIAN_POINT('Ctrl Pts',(85.4169126362828,22.7618687715364,-8.66501615063307));
#9947=CARTESIAN_POINT('Ctrl Pts',(84.1108239277452,20.8403140564757,-8.77614926862462));
#9948=CARTESIAN_POINT('Ctrl Pts',(81.7880654389434,20.8953889211715,-8.88728238661619));
#9949=CARTESIAN_POINT('Ctrl Pts',(80.958434142698,22.2498852031596,-8.96325753689542));
#9950=CARTESIAN_POINT('Ctrl Pts',(80.9419424134073,22.9647236139308,-9.0021883145108));
#9951=CARTESIAN_POINT('Ctrl Pts',(80.9420824460358,22.9993679634637,-9.00407471946233));
#9952=CARTESIAN_POINT('Ctrl Pts',(80.944726360752,22.998158663221,-8.24592528053768));
#9953=CARTESIAN_POINT('Ctrl Pts',(80.9497076461214,23.5378860633926,-8.27521534629936));
#9954=CARTESIAN_POINT('Ctrl Pts',(81.444078523515,24.7683045917449,-8.3415497847249));
#9955=CARTESIAN_POINT('Ctrl Pts',(83.5192142474232,25.3724648971313,-8.44492859581431));
#9956=CARTESIAN_POINT('Ctrl Pts',(85.2747978255561,23.850569204887,-8.55606171380586));
#9957=CARTESIAN_POINT('Ctrl Pts',(84.9483968969088,21.5501991003249,-8.66719483179741));
#9958=CARTESIAN_POINT('Ctrl Pts',(82.8387464408891,20.5767438417137,-8.77832794978898));
#9959=CARTESIAN_POINT('Ctrl Pts',(81.1984096789596,21.6170977740004,-8.87123809936906));
#9960=CARTESIAN_POINT('Ctrl Pts',(80.9487183577381,22.6516188786005,-8.92710387628529));
#9961=CARTESIAN_POINT('Ctrl Pts',(80.9485808590134,23.0000908847555,-8.94592528053767));
#9962=CARTESIAN_POINT('Origin',(83.,23.,-4.45407471946233));
#9963=CARTESIAN_POINT('',(80.9425253333126,23.001059282702,-7.54592528053768));
#9964=CARTESIAN_POINT('',(80.948463814507,22.9994822145756,-7.60407471946232));
#9965=CARTESIAN_POINT('',(80.94525,23.0000000000001,-4.45407471946233));
#9966=CARTESIAN_POINT('Ctrl Pts',(80.948463814507,22.9994822145757,-7.60407471946232));
#9967=CARTESIAN_POINT('Ctrl Pts',(80.9493091967327,23.3743099216938,-7.62432250921123));
#9968=CARTESIAN_POINT('Ctrl Pts',(81.2270644273999,24.4360706544673,-7.68161467162399));
#9969=CARTESIAN_POINT('Ctrl Pts',(82.9319188372278,25.4276610173216,-7.7759512067006));
#9970=CARTESIAN_POINT('Ctrl Pts',(85.0026324571524,24.3739128224606,-7.88708432469215));
#9971=CARTESIAN_POINT('Ctrl Pts',(85.2404580324118,22.0627054938917,-7.99821744268371));
#9972=CARTESIAN_POINT('Ctrl Pts',(83.427728231352,20.6093470098792,-8.10935056067528));
#9973=CARTESIAN_POINT('Ctrl Pts',(81.4056136835162,21.283317959634,-8.21130298626814));
#9974=CARTESIAN_POINT('Ctrl Pts',(80.9501799143854,22.4879241340947,-8.27621103919716));
#9975=CARTESIAN_POINT('Ctrl Pts',(80.9455227171961,23.0018771067991,-8.30407471946232));
#9976=CARTESIAN_POINT('Ctrl Pts',(80.9425253333126,23.001059282702,-7.54592528053768));
#9977=CARTESIAN_POINT('Ctrl Pts',(80.9421429357283,23.0619343498909,-7.54923807098573));
#9978=CARTESIAN_POINT('Ctrl Pts',(80.9722035152768,23.8031452401182,-7.58959523409763));
#9979=CARTESIAN_POINT('Ctrl Pts',(81.8697768675109,25.1495971491679,-7.66699676987337));
#9980=CARTESIAN_POINT('Ctrl Pts',(84.1929368847996,25.1154372776465,-7.77812988786495));
#9981=CARTESIAN_POINT('Ctrl Pts',(85.4242743200689,23.1451456867025,-7.8892630058565));
#9982=CARTESIAN_POINT('Ctrl Pts',(84.4368203745666,21.042011180836,-8.00039612384806));
#9983=CARTESIAN_POINT('Ctrl Pts',(82.1343319219779,20.7309050425608,-8.11152924183962));
#9984=CARTESIAN_POINT('Ctrl Pts',(81.022161499857,22.031209731433,-8.1933722940695));
#9985=CARTESIAN_POINT('Ctrl Pts',(80.9434076059279,22.8552702197982,-8.23817097363551));
#9986=CARTESIAN_POINT('Ctrl Pts',(80.944726360752,22.998158663221,-8.24592528053768));
#9987=CARTESIAN_POINT('Origin',(83.,23.,-4.45407471946233));
#9988=CARTESIAN_POINT('',(80.9479086080167,23.0011644845222,-6.84592528053768));
#9989=CARTESIAN_POINT('',(80.943624771683,22.9983937941554,-6.90407471946232));
#9990=CARTESIAN_POINT('',(80.94525,23.0000000000001,-4.45407471946233));
#9991=CARTESIAN_POINT('Ctrl Pts',(80.943624771683,22.9983937941554,-6.90407471946232));
#9992=CARTESIAN_POINT('Ctrl Pts',(80.9485745341384,23.5746341161542,-6.93538960656144));
#9993=CARTESIAN_POINT('Ctrl Pts',(81.5015293092438,24.8408721637681,-7.00374886632442));
#9994=CARTESIAN_POINT('Ctrl Pts',(83.6477355735556,25.340642018176,-7.10915249875124));
#9995=CARTESIAN_POINT('Ctrl Pts',(85.3177709360927,23.7253357071464,-7.2202856167428));
#9996=CARTESIAN_POINT('Ctrl Pts',(84.8664912980158,21.4461709704268,-7.33141873473436));
#9997=CARTESIAN_POINT('Ctrl Pts',(82.706925266015,20.5891330421716,-7.44255185272592));
#9998=CARTESIAN_POINT('Ctrl Pts',(81.1601822794663,21.6927472756777,-7.53343718096857));
#9999=CARTESIAN_POINT('Ctrl Pts',(80.9477625264739,22.6885433546059,-7.58727813654738));
#10000=CARTESIAN_POINT('Ctrl Pts',(80.948463814507,22.9994822145757,-7.60407471946232));
#10001=CARTESIAN_POINT('Ctrl Pts',(80.9479086080167,23.0011644845222,-6.84592528053768));
#10002=CARTESIAN_POINT('Ctrl Pts',(80.9465286190407,23.2671876353822,-6.86030516833594));
#10003=CARTESIAN_POINT('Ctrl Pts',(81.1181884210441,24.2168118526317,-6.91172942879806));
#10004=CARTESIAN_POINT('Ctrl Pts',(82.5507725952567,25.3866959940047,-7.00019806192404));
#10005=CARTESIAN_POINT('Ctrl Pts',(84.7614901796242,24.6719233964163,-7.11133117991558));
#10006=CARTESIAN_POINT('Ctrl Pts',(85.3600357402078,22.4269243306697,-7.22246429790715));
#10007=CARTESIAN_POINT('Ctrl Pts',(83.7985771227055,20.7064348813032,-7.33359741589871));
#10008=CARTESIAN_POINT('Ctrl Pts',(81.5745655688421,21.0738146077992,-7.44141774344221));
#10009=CARTESIAN_POINT('Ctrl Pts',(80.9464189920752,22.381215569078,-7.51219369832188));
#10010=CARTESIAN_POINT('Ctrl Pts',(80.9425253333126,23.001059282702,-7.54592528053768));
#10011=CARTESIAN_POINT('Origin',(83.,23.,-4.45407471946233));
#10012=CARTESIAN_POINT('',(80.9473274657881,22.9976809234163,-6.14592528053767));
#10013=CARTESIAN_POINT('',(80.9434277056327,23.0014963838888,-6.20407471946233));
#10014=CARTESIAN_POINT('',(80.94525,23.0000000000001,-4.45407471946233));
#10015=CARTESIAN_POINT('',(82.4698297828114,21.0148256743283,-6.));
#10016=CARTESIAN_POINT('Ctrl Pts',(82.4698297828114,21.0148256743283,-6.));
#10017=CARTESIAN_POINT('Ctrl Pts',(81.8097404375819,21.1911123142463,-6.03704437266385));
#10018=CARTESIAN_POINT('Ctrl Pts',(81.0750709872232,21.8872127590751,-6.08568613284308));
#10019=CARTESIAN_POINT('Ctrl Pts',(80.9457104606,22.7834123400653,-6.1343278930223));
#10020=CARTESIAN_POINT('Ctrl Pts',(80.9473274657881,22.9976809234163,-6.14592528053767));
#10021=CARTESIAN_POINT('',(83.531311299962,21.0112683144402,-6.));
#10022=CARTESIAN_POINT('Origin',(83.,23.,-6.));
#10023=CARTESIAN_POINT('Ctrl Pts',(83.5313119958266,21.0112661450614,-6.));
#10024=CARTESIAN_POINT('Ctrl Pts',(82.8867917747511,20.8399706654375,-6.03631814560907));
#10025=CARTESIAN_POINT('Ctrl Pts',(81.5070301779678,21.1592646346911,-6.1043430520965));
#10026=CARTESIAN_POINT('Ctrl Pts',(80.9482804526145,22.418323940505,-6.17236795858395));
#10027=CARTESIAN_POINT('Ctrl Pts',(80.9434277056327,23.0014963838888,-6.20407471946233));
#10028=CARTESIAN_POINT('Origin',(83.,-23.,-12.));
#10029=CARTESIAN_POINT('',(81.3313535412238,-23.0003916921662,-16.2285196366098));
#10030=CARTESIAN_POINT('',(81.3334663482475,-22.9985217515097,-16.4214803633902));
#10031=CARTESIAN_POINT('',(81.334,-23.,-12.));
#10032=CARTESIAN_POINT('',(82.2300979593295,-24.4774325188554,-17.));
#10033=CARTESIAN_POINT('Ctrl Pts',(81.3334663482475,-22.9985217515097,-16.4214803633902));
#10034=CARTESIAN_POINT('Ctrl Pts',(81.3324167011274,-22.8847143817383,-16.4290983789409));
#10035=CARTESIAN_POINT('Ctrl Pts',(81.3430833954876,-22.7711019357605,-16.4367163944915));
#10036=CARTESIAN_POINT('Ctrl Pts',(81.3661911854064,-22.660076333029,-16.4443344100422));
#10037=CARTESIAN_POINT('Ctrl Pts',(81.4785581890567,-22.1201885137589,-16.4813787827061));
#10038=CARTESIAN_POINT('Ctrl Pts',(81.885109434169,-21.6414696256838,-16.5184231553699));
#10039=CARTESIAN_POINT('Ctrl Pts',(82.3995342859918,-21.4430319247283,-16.5554675280338));
#10040=CARTESIAN_POINT('Ctrl Pts',(82.9139591378146,-21.2445942237728,-16.5925119006976));
#10041=CARTESIAN_POINT('Ctrl Pts',(83.5362575963479,-21.3264377099369,-16.6295562733615));
#10042=CARTESIAN_POINT('Ctrl Pts',(83.9821833263623,-21.6510262177334,-16.6666006460253));
#10043=CARTESIAN_POINT('Ctrl Pts',(84.4281090563767,-21.9756147255299,-16.7036450186892));
#10044=CARTESIAN_POINT('Ctrl Pts',(84.6976620578723,-22.5429482549589,-16.740689391353));
#10045=CARTESIAN_POINT('Ctrl Pts',(84.6664136178775,-23.09358162467,-16.7777337640169));
#10046=CARTESIAN_POINT('Ctrl Pts',(84.6351651778828,-23.6442149943811,-16.8147781366807));
#10047=CARTESIAN_POINT('Ctrl Pts',(84.3031152963976,-24.1781482043742,-16.8518225093446));
#10048=CARTESIAN_POINT('Ctrl Pts',(83.8246635830312,-24.4504525233503,-16.8888668820084));
#10049=CARTESIAN_POINT('Ctrl Pts',(83.3462118696648,-24.7227568423263,-16.9259112546723));
#10050=CARTESIAN_POINT('Ctrl Pts',(82.7213583244172,-24.7334322702853,-16.9629556273362));
#10051=CARTESIAN_POINT('Ctrl Pts',(82.2300979593296,-24.4774325188554,-17.));
#10052=CARTESIAN_POINT('',(81.662974037086,-22.0009968623267,-17.));
#10053=CARTESIAN_POINT('Origin',(83.,-23.,-17.));
#10054=CARTESIAN_POINT('',(81.3354783154905,-23.001221079894,-16.9285196366098));
#10055=CARTESIAN_POINT('Ctrl Pts',(81.6629726161761,-22.000995687242,-17.));
#10056=CARTESIAN_POINT('Ctrl Pts',(81.4510074599991,-22.2854498000758,-16.9761732122033));
#10057=CARTESIAN_POINT('Ctrl Pts',(81.3378311424635,-22.644062616804,-16.9523464244065));
#10058=CARTESIAN_POINT('Ctrl Pts',(81.3354783154905,-23.001221079894,-16.9285196366098));
#10059=CARTESIAN_POINT('',(81.334,-23.,-18.));
#10060=CARTESIAN_POINT('',(81.334,-23.,-12.));
#10061=CARTESIAN_POINT('Origin',(83.,-23.,-18.));
#10062=CARTESIAN_POINT('Ctrl Pts',(81.3354783154905,-23.001221079894,-16.9285196366098));
#10063=CARTESIAN_POINT('Ctrl Pts',(81.3342448297249,-23.1884638671393,-16.9160282787975));
#10064=CARTESIAN_POINT('Ctrl Pts',(81.3634706586964,-23.3753069321328,-16.9035369209851));
#10065=CARTESIAN_POINT('Ctrl Pts',(81.4248898698669,-23.5508552241813,-16.8910455631728));
#10066=CARTESIAN_POINT('Ctrl Pts',(81.6070346920316,-24.0714612662822,-16.8540011905089));
#10067=CARTESIAN_POINT('Ctrl Pts',(82.0723133658506,-24.492732216851,-16.8169568178451));
#10068=CARTESIAN_POINT('Ctrl Pts',(82.6082885283144,-24.6221191089392,-16.7799124451812));
#10069=CARTESIAN_POINT('Ctrl Pts',(83.1442636907781,-24.7515060010274,-16.7428680725174));
#10070=CARTESIAN_POINT('Ctrl Pts',(83.7509353418865,-24.589008834635,-16.7058236998535));
#10071=CARTESIAN_POINT('Ctrl Pts',(84.1504371851532,-24.2088727275756,-16.6687793271897));
#10072=CARTESIAN_POINT('Ctrl Pts',(84.5499390284198,-23.8287366205161,-16.6317349545258));
#10073=CARTESIAN_POINT('Ctrl Pts',(84.7422710638447,-23.2309615727897,-16.594690581862));
#10074=CARTESIAN_POINT('Ctrl Pts',(84.6395393530548,-22.6891597720865,-16.5576462091981));
#10075=CARTESIAN_POINT('Ctrl Pts',(84.536807642265,-22.1473579713834,-16.5206018365343));
#10076=CARTESIAN_POINT('Ctrl Pts',(84.1390121852604,-21.6615294177034,-16.4835574638704));
#10077=CARTESIAN_POINT('Ctrl Pts',(83.6281313466739,-21.4539694514453,-16.4465130912065));
#10078=CARTESIAN_POINT('Ctrl Pts',(83.1172505080875,-21.2464094851871,-16.4094687185427));
#10079=CARTESIAN_POINT('Ctrl Pts',(82.4932842879192,-21.3171181063508,-16.3724243458788));
#10080=CARTESIAN_POINT('Ctrl Pts',(82.0418023292256,-21.6337523848716,-16.335379973215));
#10081=CARTESIAN_POINT('Ctrl Pts',(81.6076786858952,-21.9382128930889,-16.2997598610133));
#10082=CARTESIAN_POINT('Ctrl Pts',(81.3330311221208,-22.4700521740837,-16.2641397488115));
#10083=CARTESIAN_POINT('Ctrl Pts',(81.3313535412238,-23.0003916921662,-16.2285196366098));
#10084=CARTESIAN_POINT('Origin',(83.,-23.,-12.));
#10085=CARTESIAN_POINT('',(81.3344265803655,-22.9984874575686,-15.5285196366098));
#10086=CARTESIAN_POINT('',(81.3367022463126,-23.0000402080689,-15.7214803633902));
#10087=CARTESIAN_POINT('',(81.334,-23.,-12.));
#10088=CARTESIAN_POINT('Ctrl Pts',(81.3367022463126,-23.0000402080689,-15.7214803633902));
#10089=CARTESIAN_POINT('Ctrl Pts',(81.3367622607545,-22.7195427638815,-15.7401654762911));
#10090=CARTESIAN_POINT('Ctrl Pts',(81.403932944649,-22.4390181888952,-15.758850589192));
#10091=CARTESIAN_POINT('Ctrl Pts',(81.5380528521339,-22.1953422621795,-15.7775357020929));
#10092=CARTESIAN_POINT('Ctrl Pts',(81.8039537252442,-21.7122399182789,-15.8145800747567));
#10093=CARTESIAN_POINT('Ctrl Pts',(82.3330016941159,-21.373972932507,-15.8516244474206));
#10094=CARTESIAN_POINT('Ctrl Pts',(82.8830897925016,-21.3353395855451,-15.8886688200844));
#10095=CARTESIAN_POINT('Ctrl Pts',(83.4331778908874,-21.2967062385831,-15.9257131927483));
#10096=CARTESIAN_POINT('Ctrl Pts',(84.0043061187875,-21.5577065304311,-15.9627575654121));
#10097=CARTESIAN_POINT('Ctrl Pts',(84.33512334448,-21.9989002927704,-15.999801938076));
#10098=CARTESIAN_POINT('Ctrl Pts',(84.6659405701726,-22.4400940551098,-16.0368463107398));
#10099=CARTESIAN_POINT('Ctrl Pts',(84.7564467936577,-23.0614812879405,-16.0738906834037));
#10100=CARTESIAN_POINT('Ctrl Pts',(84.5652078620693,-23.5787055542428,-16.1109350560675));
#10101=CARTESIAN_POINT('Ctrl Pts',(84.3739689304809,-24.0959298205451,-16.1479794287314));
#10102=CARTESIAN_POINT('Ctrl Pts',(83.9009848438189,-24.508991120319,-16.1850238013952));
#10103=CARTESIAN_POINT('Ctrl Pts',(83.3627357838583,-24.6288593090619,-16.2220681740591));
#10104=CARTESIAN_POINT('Ctrl Pts',(82.8244867238977,-24.7487274978049,-16.2591125467229));
#10105=CARTESIAN_POINT('Ctrl Pts',(82.2209726906385,-24.575402575517,-16.2961569193868));
#10106=CARTESIAN_POINT('Ctrl Pts',(81.828307055103,-24.1882117391405,-16.3332012920507));
#10107=CARTESIAN_POINT('Ctrl Pts',(81.5163914148467,-23.8806450291963,-16.3626276491638));
#10108=CARTESIAN_POINT('Ctrl Pts',(81.3375208544104,-23.4381291903146,-16.392054006277));
#10109=CARTESIAN_POINT('Ctrl Pts',(81.3334663482475,-22.9985217515097,-16.4214803633902));
#10110=CARTESIAN_POINT('Ctrl Pts',(81.3313535412238,-23.0003916921662,-16.2285196366098));
#10111=CARTESIAN_POINT('Ctrl Pts',(81.3312864636096,-23.0215971730145,-16.2270953761477));
#10112=CARTESIAN_POINT('Ctrl Pts',(81.3316558045061,-23.0428002560741,-16.2256711156856));
#10113=CARTESIAN_POINT('Ctrl Pts',(81.3324688192059,-23.0639863098917,-16.2242468552234));
#10114=CARTESIAN_POINT('Ctrl Pts',(81.3536149650986,-23.6150260205131,-16.1872024825596));
#10115=CARTESIAN_POINT('Ctrl Pts',(81.6749049541029,-24.1545455058778,-16.1501581098957));
#10116=CARTESIAN_POINT('Ctrl Pts',(82.1493178143438,-24.4356537351314,-16.1131137372319));
#10117=CARTESIAN_POINT('Ctrl Pts',(82.6237306745847,-24.716761964385,-16.076069364568));
#10118=CARTESIAN_POINT('Ctrl Pts',(83.2512664060623,-24.7394589375276,-16.0390249919042));
#10119=CARTESIAN_POINT('Ctrl Pts',(83.7447484720246,-24.4933562158936,-16.0019806192403));
#10120=CARTESIAN_POINT('Ctrl Pts',(84.2382305379868,-24.2472534942596,-15.9649362465765));
#10121=CARTESIAN_POINT('Ctrl Pts',(84.5976589384339,-23.7323510778492,-15.9278918739126));
#10122=CARTESIAN_POINT('Ctrl Pts',(84.6585540875959,-23.1842793768616,-15.8908475012488));
#10123=CARTESIAN_POINT('Ctrl Pts',(84.7194492367579,-22.6362076758741,-15.8538031285849));
#10124=CARTESIAN_POINT('Ctrl Pts',(84.4818111346349,-22.0549666903095,-15.8167587559211));
#10125=CARTESIAN_POINT('Ctrl Pts',(84.0543866887268,-21.706543266871,-15.7797143832572));
#10126=CARTESIAN_POINT('Ctrl Pts',(83.6269622428187,-21.3581198434324,-15.7426700105933));
#10127=CARTESIAN_POINT('Ctrl Pts',(83.0097514531255,-21.2425139821199,-15.7056256379295));
#10128=CARTESIAN_POINT('Ctrl Pts',(82.4852026073696,-21.4126294343583,-15.6685812652656));
#10129=CARTESIAN_POINT('Ctrl Pts',(81.9606537616137,-21.5827448865967,-15.6315368926018));
#10130=CARTESIAN_POINT('Ctrl Pts',(81.5287668597951,-22.0385816523861,-15.5944925199379));
#10131=CARTESIAN_POINT('Ctrl Pts',(81.3871816050425,-22.5715397394835,-15.5574481472741));
#10132=CARTESIAN_POINT('Ctrl Pts',(81.3503262497169,-22.7102714153768,-15.547805310386));
#10133=CARTESIAN_POINT('Ctrl Pts',(81.3331413605435,-22.8542287327907,-15.5381624734979));
#10134=CARTESIAN_POINT('Ctrl Pts',(81.3344265803655,-22.9984874575686,-15.5285196366098));
#10135=CARTESIAN_POINT('Origin',(83.,-23.,-12.));
#10136=CARTESIAN_POINT('',(81.3365469135995,-23.0005281518415,-14.8285196366098));
#10137=CARTESIAN_POINT('',(81.3333662687744,-23.0014645813323,-15.0214803633902));
#10138=CARTESIAN_POINT('',(81.334,-23.,-12.));
#10139=CARTESIAN_POINT('Ctrl Pts',(81.3333662687744,-23.0014645813323,-15.0214803633902));
#10140=CARTESIAN_POINT('Ctrl Pts',(81.3374449537321,-22.5570899997421,-15.0512325736413));
#10141=CARTESIAN_POINT('Ctrl Pts',(81.5206881577281,-22.1097458291912,-15.0809847838924));
#10142=CARTESIAN_POINT('Ctrl Pts',(81.8387594570367,-21.8015500092252,-15.1107369941435));
#10143=CARTESIAN_POINT('Ctrl Pts',(82.2347889165566,-21.4178164744086,-15.1477813668074));
#10144=CARTESIAN_POINT('Ctrl Pts',(82.839837690827,-21.249799796086,-15.1848257394712));
#10145=CARTESIAN_POINT('Ctrl Pts',(83.3770234867105,-21.3743877231352,-15.2218701121351));
#10146=CARTESIAN_POINT('Ctrl Pts',(83.914209282594,-21.4989756501844,-15.2589144847989));
#10147=CARTESIAN_POINT('Ctrl Pts',(84.3835321000906,-21.9161681826054,-15.2959588574628));
#10148=CARTESIAN_POINT('Ctrl Pts',(84.5702207149372,-22.4350497866678,-15.3330032301266));
#10149=CARTESIAN_POINT('Ctrl Pts',(84.7569093297838,-22.9539313907302,-15.3700476027905));
#10150=CARTESIAN_POINT('Ctrl Pts',(84.6609637419804,-23.5745020664339,-15.4070919754543));
#10151=CARTESIAN_POINT('Ctrl Pts',(84.3262902750188,-24.0127765010024,-15.4441363481182));
#10152=CARTESIAN_POINT('Ctrl Pts',(83.9916168080572,-24.4510509355709,-15.481180720782));
#10153=CARTESIAN_POINT('Ctrl Pts',(83.4182154619373,-24.7070291290041,-15.5182250934459));
#10154=CARTESIAN_POINT('Ctrl Pts',(82.8684865069619,-24.6635703403376,-15.5552694661097));
#10155=CARTESIAN_POINT('Ctrl Pts',(82.3187575519866,-24.6201115516712,-15.5923138387736));
#10156=CARTESIAN_POINT('Ctrl Pts',(81.7927009881558,-24.2772157809052,-15.6293582114374));
#10157=CARTESIAN_POINT('Ctrl Pts',(81.5310495949151,-23.7917990445074,-15.6664025841013));
#10158=CARTESIAN_POINT('Ctrl Pts',(81.4013746793903,-23.5512256101106,-15.6847618438643));
#10159=CARTESIAN_POINT('Ctrl Pts',(81.3366432784737,-23.2756460054758,-15.7031211036272));
#10160=CARTESIAN_POINT('Ctrl Pts',(81.3367022463126,-23.0000402080689,-15.7214803633902));
#10161=CARTESIAN_POINT('Ctrl Pts',(81.3344265803655,-22.9984874575686,-15.5285196366098));
#10162=CARTESIAN_POINT('Ctrl Pts',(81.3380787210521,-23.4084197890849,-15.501118100834));
#10163=CARTESIAN_POINT('Ctrl Pts',(81.4908761802709,-23.820785971822,-15.4737165650583));
#10164=CARTESIAN_POINT('Ctrl Pts',(81.7652753558034,-24.1225936800591,-15.4463150292825));
#10165=CARTESIAN_POINT('Ctrl Pts',(82.1362379690038,-24.5306101251318,-15.4092706566187));
#10166=CARTESIAN_POINT('Ctrl Pts',(82.7294468030913,-24.7365636068717,-15.3722262839548));
#10167=CARTESIAN_POINT('Ctrl Pts',(83.2734377603458,-24.6462057293775,-15.335181911291));
#10168=CARTESIAN_POINT('Ctrl Pts',(83.8174287176003,-24.5558478518833,-15.2981375386271));
#10169=CARTESIAN_POINT('Ctrl Pts',(84.3122017980218,-24.1691786151549,-15.2610931659633));
#10170=CARTESIAN_POINT('Ctrl Pts',(84.5313391335624,-23.6631454863052,-15.2240487932994));
#10171=CARTESIAN_POINT('Ctrl Pts',(84.7504764691031,-23.1571123574555,-15.1870044206356));
#10172=CARTESIAN_POINT('Ctrl Pts',(84.6939780597629,-22.5317153364845,-15.1499600479717));
#10173=CARTESIAN_POINT('Ctrl Pts',(84.3876986741927,-22.0731484004554,-15.1129156753078));
#10174=CARTESIAN_POINT('Ctrl Pts',(84.0814192886225,-21.6145814644263,-15.075871302644));
#10175=CARTESIAN_POINT('Ctrl Pts',(83.5253589268223,-21.3228446133391,-15.0388269299802));
#10176=CARTESIAN_POINT('Ctrl Pts',(82.9739817612062,-21.3314423753008,-15.0017825573163));
#10177=CARTESIAN_POINT('Ctrl Pts',(82.4226045955901,-21.3400401372625,-14.9647381846524));
#10178=CARTESIAN_POINT('Ctrl Pts',(81.8759106261582,-21.6489725122731,-14.9276938119886));
#10179=CARTESIAN_POINT('Ctrl Pts',(81.5840777682971,-22.1168659639303,-14.8906494393247));
#10180=CARTESIAN_POINT('Ctrl Pts',(81.4209264214049,-22.3784453056102,-14.8699395050864));
#10181=CARTESIAN_POINT('Ctrl Pts',(81.3374307130897,-22.6897071821857,-14.8492295708481));
#10182=CARTESIAN_POINT('Ctrl Pts',(81.3365469135995,-23.0005281518415,-14.8285196366098));
#10183=CARTESIAN_POINT('Origin',(83.,-23.,-12.));
#10184=CARTESIAN_POINT('',(81.3324918741766,-23.0012330300494,-14.1285196366098));
#10185=CARTESIAN_POINT('',(81.3319380386485,-22.9990409236778,-14.3214803633902));
#10186=CARTESIAN_POINT('',(81.334,-23.,-12.));
#10187=CARTESIAN_POINT('Ctrl Pts',(81.3319380386485,-22.9990409236778,-14.3214803633902));
#10188=CARTESIAN_POINT('Ctrl Pts',(81.3315519386774,-22.9427845253567,-14.3252552983277));
#10189=CARTESIAN_POINT('Ctrl Pts',(81.3341512567505,-22.8865642275187,-14.3290302332651));
#10190=CARTESIAN_POINT('Ctrl Pts',(81.3398535979727,-22.8306604466783,-14.3328051682026));
#10191=CARTESIAN_POINT('Ctrl Pts',(81.3958120864737,-22.2820627820619,-14.3698495408664));
#10192=CARTESIAN_POINT('Ctrl Pts',(81.750591195306,-21.7639456524137,-14.4068939135303));
#10193=CARTESIAN_POINT('Ctrl Pts',(82.241837022815,-21.5134096526244,-14.4439382861942));
#10194=CARTESIAN_POINT('Ctrl Pts',(82.733082850324,-21.262873652835,-14.480982658858));
#10195=CARTESIAN_POINT('Ctrl Pts',(83.3607953965097,-21.2799187829043,-14.5180270315219));
#10196=CARTESIAN_POINT('Ctrl Pts',(83.837721045914,-21.556744856032,-14.5550714041857));
#10197=CARTESIAN_POINT('Ctrl Pts',(84.3146466953183,-21.8335709291597,-14.5921157768496));
#10198=CARTESIAN_POINT('Ctrl Pts',(84.6407854479411,-22.3701779453458,-14.6291601495134));
#10199=CARTESIAN_POINT('Ctrl Pts',(84.6668897943504,-22.9210039733326,-14.6662045221773));
#10200=CARTESIAN_POINT('Ctrl Pts',(84.6929941407597,-23.4718300013195,-14.7032488948411));
#10201=CARTESIAN_POINT('Ctrl Pts',(84.4190640809555,-24.0368750411072,-14.740293267505));
#10202=CARTESIAN_POINT('Ctrl Pts',(83.9704553969745,-24.3575633631643,-14.7773376401688));
#10203=CARTESIAN_POINT('Ctrl Pts',(83.5218467129935,-24.6782516852214,-14.8143820128327));
#10204=CARTESIAN_POINT('Ctrl Pts',(82.8985594048357,-24.754583289548,-14.8514263854965));
#10205=CARTESIAN_POINT('Ctrl Pts',(82.3858220193069,-24.5516273305094,-14.8884707581604));
#10206=CARTESIAN_POINT('Ctrl Pts',(81.873084633778,-24.3486713714708,-14.9255151308242));
#10207=CARTESIAN_POINT('Ctrl Pts',(81.4708971708781,-23.8664278490671,-14.9625595034881));
#10208=CARTESIAN_POINT('Ctrl Pts',(81.3633085118128,-23.3255808922099,-14.9996038761519));
#10209=CARTESIAN_POINT('Ctrl Pts',(81.342129749176,-23.2191154950054,-15.0068960385647));
#10210=CARTESIAN_POINT('Ctrl Pts',(81.3323665973923,-23.1103792331753,-15.0141882009775));
#10211=CARTESIAN_POINT('Ctrl Pts',(81.3333662687744,-23.0014645813323,-15.0214803633902));
#10212=CARTESIAN_POINT('Ctrl Pts',(81.3365469135995,-23.0005281518415,-14.8285196366098));
#10213=CARTESIAN_POINT('Ctrl Pts',(81.3358498390368,-23.2456803542478,-14.8121851981843));
#10214=CARTESIAN_POINT('Ctrl Pts',(81.3865445413348,-23.4905582742853,-14.7958507597587));
#10215=CARTESIAN_POINT('Ctrl Pts',(81.4900815300601,-23.7105685812494,-14.7795163213332));
#10216=CARTESIAN_POINT('Ctrl Pts',(81.7248898959745,-24.2095232186075,-14.7424719486693));
#10217=CARTESIAN_POINT('Ctrl Pts',(82.2314783740936,-24.5805779650201,-14.7054275760055));
#10218=CARTESIAN_POINT('Ctrl Pts',(82.778022106296,-24.6539308657728,-14.6683832033416));
#10219=CARTESIAN_POINT('Ctrl Pts',(83.3245658384983,-24.7272837665254,-14.6313388306778));
#10220=CARTESIAN_POINT('Ctrl Pts',(83.9110648247838,-24.5029348216182,-14.5942944580139));
#10221=CARTESIAN_POINT('Ctrl Pts',(84.2691255873272,-24.0835505236204,-14.55725008535));
#10222=CARTESIAN_POINT('Ctrl Pts',(84.6271863498705,-23.6641662256226,-14.5202057126862));
#10223=CARTESIAN_POINT('Ctrl Pts',(84.7568088886717,-23.0497465745342,-14.4831613400223));
#10224=CARTESIAN_POINT('Ctrl Pts',(84.5986753787846,-22.521462094236,-14.4461169673585));
#10225=CARTESIAN_POINT('Ctrl Pts',(84.4405418688976,-21.9931776139378,-14.4090725946946));
#10226=CARTESIAN_POINT('Ctrl Pts',(83.9946523103222,-21.5510283044299,-14.3720282220308));
#10227=CARTESIAN_POINT('Ctrl Pts',(83.465054540206,-21.3973503912159,-14.3349838493669));
#10228=CARTESIAN_POINT('Ctrl Pts',(82.9354567700899,-21.2436724780019,-14.2979394767031));
#10229=CARTESIAN_POINT('Ctrl Pts',(82.3221507884329,-21.3784659610818,-14.2608951040392));
#10230=CARTESIAN_POINT('Ctrl Pts',(81.9057974821241,-21.7400466898587,-14.2238507313754));
#10231=CARTESIAN_POINT('Ctrl Pts',(81.5486454718412,-22.0502142379612,-14.1920736997868));
#10232=CARTESIAN_POINT('Ctrl Pts',(81.3364187077672,-22.5272604403474,-14.1602966681983));
#10233=CARTESIAN_POINT('Ctrl Pts',(81.3324918741766,-23.0012330300494,-14.1285196366098));
#10234=CARTESIAN_POINT('Origin',(83.,-23.,-12.));
#10235=CARTESIAN_POINT('',(81.3327118147905,-22.9986896254657,-13.4285196366098));
#10236=CARTESIAN_POINT('',(81.3362661410155,-22.99914450019,-13.6214803633902));
#10237=CARTESIAN_POINT('',(81.334,-23.,-12.));
#10238=CARTESIAN_POINT('Ctrl Pts',(81.3362661410155,-22.99914450019,-13.6214803633902));
#10239=CARTESIAN_POINT('Ctrl Pts',(81.3352300865187,-22.776484691814,-13.6363223956779));
#10240=CARTESIAN_POINT('Ctrl Pts',(81.376782632399,-22.5541957175097,-13.6511644279656));
#10241=CARTESIAN_POINT('Ctrl Pts',(81.4627522870129,-22.3506684747836,-13.6660064602532));
#10242=CARTESIAN_POINT('Ctrl Pts',(81.6773247836614,-21.8426828512073,-13.7030508329171));
#10243=CARTESIAN_POINT('Ctrl Pts',(82.1685965611403,-21.4515746602874,-13.7400952055809));
#10244=CARTESIAN_POINT('Ctrl Pts',(82.7117519859494,-21.3563227071218,-13.7771395782448));
#10245=CARTESIAN_POINT('Ctrl Pts',(83.2549074107585,-21.2610707539562,-13.8141839509087));
#10246=CARTESIAN_POINT('Ctrl Pts',(83.8499464828978,-21.4616750385448,-13.8512283235725));
#10247=CARTESIAN_POINT('Ctrl Pts',(84.2245676126847,-21.8663350924087,-13.8882726962364));
#10248=CARTESIAN_POINT('Ctrl Pts',(84.5991887424716,-22.2709951462725,-13.9253170689002));
#10249=CARTESIAN_POINT('Ctrl Pts',(84.7533919299061,-22.8797109694116,-13.9623614415641));
#10250=CARTESIAN_POINT('Ctrl Pts',(84.6166107617626,-23.4139222217417,-13.9994058142279));
#10251=CARTESIAN_POINT('Ctrl Pts',(84.479829593619,-23.9481334740717,-14.0364501868918));
#10252=CARTESIAN_POINT('Ctrl Pts',(84.0520640698975,-24.4078401555926,-14.0734945595556));
#10253=CARTESIAN_POINT('Ctrl Pts',(83.5290681125294,-24.5826714419116,-14.1105389322195));
#10254=CARTESIAN_POINT('Ctrl Pts',(83.0060721551613,-24.7575027282305,-14.1475833048833));
#10255=CARTESIAN_POINT('Ctrl Pts',(82.3878457641466,-24.6474586193474,-14.1846276775472));
#10256=CARTESIAN_POINT('Ctrl Pts',(81.9573015027242,-24.3028974651135,-14.221672050211));
#10257=CARTESIAN_POINT('Ctrl Pts',(81.5706310190902,-23.9934481469204,-14.2549414879374));
#10258=CARTESIAN_POINT('Ctrl Pts',(81.3353408334404,-23.4948425127546,-14.2882109256638));
#10259=CARTESIAN_POINT('Ctrl Pts',(81.3319380386485,-22.9990409236778,-14.3214803633902));
#10260=CARTESIAN_POINT('Ctrl Pts',(81.3324918741766,-23.0012330300494,-14.1285196366098));
#10261=CARTESIAN_POINT('Ctrl Pts',(81.3318409646726,-23.0797984329682,-14.1232522955345));
#10262=CARTESIAN_POINT('Ctrl Pts',(81.3369133399439,-23.1582793847753,-14.1179849544591));
#10263=CARTESIAN_POINT('Ctrl Pts',(81.3479976357627,-23.2359018492069,-14.1127176133838));
#10264=CARTESIAN_POINT('Ctrl Pts',(81.4259517266709,-23.7818083053044,-14.07567324072));
#10265=CARTESIAN_POINT('Ctrl Pts',(81.801260539448,-24.2852532430257,-14.0386288680561));
#10266=CARTESIAN_POINT('Ctrl Pts',(82.3021753753463,-24.5158503511622,-14.0015844953923));
#10267=CARTESIAN_POINT('Ctrl Pts',(82.8030902112445,-24.7464474592986,-13.9645401227284));
#10268=CARTESIAN_POINT('Ctrl Pts',(83.429611070264,-24.7041967378502,-13.9274957500646));
#10269=CARTESIAN_POINT('Ctrl Pts',(83.8950296775147,-24.4084329484417,-13.8904513774007));
#10270=CARTESIAN_POINT('Ctrl Pts',(84.3604482847654,-24.1126691590331,-13.8534070047368));
#10271=CARTESIAN_POINT('Ctrl Pts',(84.6647646402474,-23.5633923016643,-13.816362632073));
#10272=CARTESIAN_POINT('Ctrl Pts',(84.6687175908008,-23.0119622759285,-13.7793182594091));
#10273=CARTESIAN_POINT('Ctrl Pts',(84.6726705413541,-22.4605322501928,-13.7422738867453));
#10274=CARTESIAN_POINT('Ctrl Pts',(84.3762600869788,-21.9069490560902,-13.7052295140814));
#10275=CARTESIAN_POINT('Ctrl Pts',(83.9151294848998,-21.6045432576541,-13.6681851414176));
#10276=CARTESIAN_POINT('Ctrl Pts',(83.4539988828207,-21.302137459218,-13.6311407687537));
#10277=CARTESIAN_POINT('Ctrl Pts',(82.8281481330379,-21.2509090564484,-13.5940963960899));
#10278=CARTESIAN_POINT('Ctrl Pts',(82.3239788552738,-21.4743011746173,-13.557052023426));
#10279=CARTESIAN_POINT('Ctrl Pts',(81.8198095775097,-21.6976932927862,-13.5200076507622));
#10280=CARTESIAN_POINT('Ctrl Pts',(81.4373217717644,-22.1957059318936,-13.4829632780983));
#10281=CARTESIAN_POINT('Ctrl Pts',(81.3515493852339,-22.7404387074911,-13.4459189054345));
#10282=CARTESIAN_POINT('Ctrl Pts',(81.3381206536555,-22.825723383846,-13.4401191491596));
#10283=CARTESIAN_POINT('Ctrl Pts',(81.3319649476304,-22.9121532542978,-13.4343193928847));
#10284=CARTESIAN_POINT('Ctrl Pts',(81.3327118147905,-22.9986896254657,-13.4285196366098));
#10285=CARTESIAN_POINT('Origin',(83.,-23.,-12.));
#10286=CARTESIAN_POINT('',(81.3366136549425,-22.9995968836278,-12.7285196366098));
#10287=CARTESIAN_POINT('',(81.3350587862692,-23.0014219189523,-12.9214803633902));
#10288=CARTESIAN_POINT('',(81.334,-23.,-12.));
#10289=CARTESIAN_POINT('Ctrl Pts',(81.3350587862692,-23.0014219189523,-12.9214803633902));
#10290=CARTESIAN_POINT('Ctrl Pts',(81.3382109857955,-22.613442580851,-12.9473894930281));
#10291=CARTESIAN_POINT('Ctrl Pts',(81.4733906271644,-22.2234832157686,-12.973298622666));
#10292=CARTESIAN_POINT('Ctrl Pts',(81.7211701893928,-21.9279196502921,-12.9992077523039));
#10293=CARTESIAN_POINT('Ctrl Pts',(82.0754406172289,-21.5053285784039,-13.0362521249677));
#10294=CARTESIAN_POINT('Ctrl Pts',(82.6598959956844,-21.2757082679968,-13.0732964976316));
#10295=CARTESIAN_POINT('Ctrl Pts',(83.2070780416085,-21.3441374919967,-13.1103408702954));
#10296=CARTESIAN_POINT('Ctrl Pts',(83.7542600875325,-21.4125667159967,-13.1473852429593));
#10297=CARTESIAN_POINT('Ctrl Pts',(84.2641688009252,-21.7790454744038,-13.1844296156232));
#10298=CARTESIAN_POINT('Ctrl Pts',(84.5034599196319,-22.2758658751392,-13.221473988287));
#10299=CARTESIAN_POINT('Ctrl Pts',(84.7427510383386,-22.7726862758745,-13.2585183609509));
#10300=CARTESIAN_POINT('Ctrl Pts',(84.7114245623595,-23.3998483189383,-13.2955627336147));
#10301=CARTESIAN_POINT('Ctrl Pts',(84.4238161036021,-23.8703503109956,-13.3326071062786));
#10302=CARTESIAN_POINT('Ctrl Pts',(84.1362076448448,-24.340852303053,-13.3696514789424));
#10303=CARTESIAN_POINT('Ctrl Pts',(83.5923172033091,-24.6546942441039,-13.4066958516063));
#10304=CARTESIAN_POINT('Ctrl Pts',(83.0410397487005,-24.6682558855744,-13.4437402242701));
#10305=CARTESIAN_POINT('Ctrl Pts',(82.4897622940919,-24.681817527045,-13.480784596934));
#10306=CARTESIAN_POINT('Ctrl Pts',(81.9310978264102,-24.3950988689351,-13.5178289695978));
#10307=CARTESIAN_POINT('Ctrl Pts',(81.6207022004784,-23.9393080117639,-13.5548733422617));
#10308=CARTESIAN_POINT('Ctrl Pts',(81.4346682945799,-23.6661322761914,-13.5770756826379));
#10309=CARTESIAN_POINT('Ctrl Pts',(81.3378159850085,-23.3322234719803,-13.599278023014));
#10310=CARTESIAN_POINT('Ctrl Pts',(81.3362661410155,-22.99914450019,-13.6214803633902));
#10311=CARTESIAN_POINT('Ctrl Pts',(81.3327118147905,-22.9986896254657,-13.4285196366098));
#10312=CARTESIAN_POINT('Ctrl Pts',(81.3367353593684,-23.4648808915603,-13.3972750202208));
#10313=CARTESIAN_POINT('Ctrl Pts',(81.5410870292824,-23.9341630468355,-13.3660304038319));
#10314=CARTESIAN_POINT('Ctrl Pts',(81.887846800212,-24.2441369515021,-13.3347857874429));
#10315=CARTESIAN_POINT('Ctrl Pts',(82.2989735690362,-24.6116495078282,-13.297741414779));
#10316=CARTESIAN_POINT('Ctrl Pts',(82.9102840740004,-24.7552217083932,-13.2606970421152));
#10317=CARTESIAN_POINT('Ctrl Pts',(83.4420305975594,-24.6091520887451,-13.2236526694514));
#10318=CARTESIAN_POINT('Ctrl Pts',(83.9737771211185,-24.463082469097,-13.1866082967875));
#10319=CARTESIAN_POINT('Ctrl Pts',(84.4259596632723,-24.0273710292358,-13.1495639241236));
#10320=CARTESIAN_POINT('Ctrl Pts',(84.5916505938657,-23.5014078987596,-13.1125195514598));
#10321=CARTESIAN_POINT('Ctrl Pts',(84.757341524459,-22.9754447682834,-13.0754751787959));
#10322=CARTESIAN_POINT('Ctrl Pts',(84.636540843492,-22.3592299471921,-13.0384308061321));
#10323=CARTESIAN_POINT('Ctrl Pts',(84.2845293199092,-21.9347554646067,-13.0013864334682));
#10324=CARTESIAN_POINT('Ctrl Pts',(83.9325177963264,-21.5102809820213,-12.9643420608044));
#10325=CARTESIAN_POINT('Ctrl Pts',(83.3492954301278,-21.2775468379417,-12.9272976881405));
#10326=CARTESIAN_POINT('Ctrl Pts',(82.8017562537904,-21.3430567568621,-12.8902533154767));
#10327=CARTESIAN_POINT('Ctrl Pts',(82.2542170774529,-21.4085666757825,-12.8532089428128));
#10328=CARTESIAN_POINT('Ctrl Pts',(81.7423610909766,-21.7723206577029,-12.816164570149));
#10329=CARTESIAN_POINT('Ctrl Pts',(81.5004236670005,-22.2678577218878,-12.7791201974851));
#10330=CARTESIAN_POINT('Ctrl Pts',(81.3902659608985,-22.4934831145288,-12.76225334386));
#10331=CARTESIAN_POINT('Ctrl Pts',(81.3360655115292,-22.7464286725523,-12.7453864902349));
#10332=CARTESIAN_POINT('Ctrl Pts',(81.3366136549425,-22.9995968836278,-12.7285196366098));
#10333=CARTESIAN_POINT('Origin',(83.,-23.,-12.));
#10334=CARTESIAN_POINT('',(81.3341897502355,-23.0015225987737,-12.0285196366098));
#10335=CARTESIAN_POINT('',(81.3312395632066,-23.0000189542825,-12.2214803633902));
#10336=CARTESIAN_POINT('',(81.334,-23.,-12.));
#10337=CARTESIAN_POINT('Ctrl Pts',(81.3312396675144,-23.0000189535663,-12.2214803633902));
#10338=CARTESIAN_POINT('Ctrl Pts',(81.3313322263269,-22.4495888888226,-12.2584565903783));
#10339=CARTESIAN_POINT('Ctrl Pts',(81.6304402577157,-21.8990726361851,-12.2954328173664));
#10340=CARTESIAN_POINT('Ctrl Pts',(82.0923259468198,-21.5996822596601,-12.3324090443545));
#10341=CARTESIAN_POINT('Ctrl Pts',(82.5550628723794,-21.2997401189022,-12.3694534170184));
#10342=CARTESIAN_POINT('Ctrl Pts',(83.1811779936747,-21.2518503366662,-12.4064977896822));
#10343=CARTESIAN_POINT('Ctrl Pts',(83.6841487093753,-21.4779282197651,-12.4435421623461));
#10344=CARTESIAN_POINT('Ctrl Pts',(84.1871194250758,-21.704006102864,-12.4805865350099));
#10345=CARTESIAN_POINT('Ctrl Pts',(84.5669457351817,-22.2040516512977,-12.5176309076738));
#10346=CARTESIAN_POINT('Ctrl Pts',(84.6498116452796,-22.7492341813025,-12.5546752803377));
#10347=CARTESIAN_POINT('Ctrl Pts',(84.7326775553775,-23.2944167113074,-12.5917196530015));
#10348=CARTESIAN_POINT('Ctrl Pts',(84.5185830654674,-23.8847362228833,-12.6287640256654));
#10349=CARTESIAN_POINT('Ctrl Pts',(84.1055020274706,-24.2500508901584,-12.6658083983292));
#10350=CARTESIAN_POINT('Ctrl Pts',(83.6924209894737,-24.6153655574334,-12.7028527709931));
#10351=CARTESIAN_POINT('Ctrl Pts',(83.0803534033903,-24.7556753804077,-12.7398971436569));
#10352=CARTESIAN_POINT('Ctrl Pts',(82.5493934419846,-24.6067718228176,-12.7769415163208));
#10353=CARTESIAN_POINT('Ctrl Pts',(82.018433480579,-24.4578682652276,-12.8139858889846));
#10354=CARTESIAN_POINT('Ctrl Pts',(81.5685811438512,-24.0197513270734,-12.8510302616485));
#10355=CARTESIAN_POINT('Ctrl Pts',(81.4056977140957,-23.4929119413115,-12.8880746343123));
#10356=CARTESIAN_POINT('Ctrl Pts',(81.3567362539654,-23.3345482230394,-12.8992098773383));
#10357=CARTESIAN_POINT('Ctrl Pts',(81.3337040318532,-23.1681679377955,-12.9103451203643));
#10358=CARTESIAN_POINT('Ctrl Pts',(81.3350587862692,-23.0014219189523,-12.9214803633902));
#10359=CARTESIAN_POINT('Ctrl Pts',(81.3366136549425,-22.9995968836278,-12.7285196366098));
#10360=CARTESIAN_POINT('Ctrl Pts',(81.3372693892249,-23.3024575423211,-12.708342117571));
#10361=CARTESIAN_POINT('Ctrl Pts',(81.4162753651713,-23.6056368378878,-12.6881645985323));
#10362=CARTESIAN_POINT('Ctrl Pts',(81.571562362921,-23.8627441166811,-12.6679870794935));
#10363=CARTESIAN_POINT('Ctrl Pts',(81.8566573442934,-24.3347733008397,-12.6309427068297));
#10364=CARTESIAN_POINT('Ctrl Pts',(82.398866168514,-24.6515115227075,-12.5938983341658));
#10365=CARTESIAN_POINT('Ctrl Pts',(82.9500634070537,-24.6680131386102,-12.556853961502));
#10366=CARTESIAN_POINT('Ctrl Pts',(83.5012606455935,-24.684514754513,-12.5198095888381));
#10367=CARTESIAN_POINT('Ctrl Pts',(84.0614462984525,-24.4007797644507,-12.4827652161743));
#10368=CARTESIAN_POINT('Ctrl Pts',(84.3742683865361,-23.946650883726,-12.4457208435104));
#10369=CARTESIAN_POINT('Ctrl Pts',(84.6870904746197,-23.4925220030013,-12.4086764708466));
#10370=CARTESIAN_POINT('Ctrl Pts',(84.752548997928,-22.8679992316143,-12.3716320981827));
#10371=CARTESIAN_POINT('Ctrl Pts',(84.5406888479839,-22.35887648024,-12.3345877255189));
#10372=CARTESIAN_POINT('Ctrl Pts',(84.3288286980399,-21.8497537288657,-12.297543352855));
#10373=CARTESIAN_POINT('Ctrl Pts',(83.8396498748435,-21.4560309975041,-12.2604989801912));
#10374=CARTESIAN_POINT('Ctrl Pts',(83.2970102348348,-21.3578835564142,-12.2234546075273));
#10375=CARTESIAN_POINT('Ctrl Pts',(82.7543705948261,-21.2597361153243,-12.1864102348635));
#10376=CARTESIAN_POINT('Ctrl Pts',(82.1582701380051,-21.457163964506,-12.1493658621996));
#10377=CARTESIAN_POINT('Ctrl Pts',(81.7814961645559,-21.8598202348316,-12.1123214895357));
#10378=CARTESIAN_POINT('Ctrl Pts',(81.4973832225279,-22.163450171212,-12.0843875385604));
#10379=CARTESIAN_POINT('Ctrl Pts',(81.3379831636485,-22.5837765854249,-12.0564535875851));
#10380=CARTESIAN_POINT('Ctrl Pts',(81.3341897502355,-23.0015225987737,-12.0285196366098));
#10381=CARTESIAN_POINT('Origin',(83.,-23.,-12.));
#10382=CARTESIAN_POINT('',(81.3314457178217,-22.9994693778887,-11.3285196366098));
#10383=CARTESIAN_POINT('',(81.3350035286226,-22.9985661148555,-11.5214803633902));
#10384=CARTESIAN_POINT('',(81.334,-23.,-12.));
#10385=CARTESIAN_POINT('Ctrl Pts',(81.3350035286226,-22.9985661148555,-11.5214803633902));
#10386=CARTESIAN_POINT('Ctrl Pts',(81.3336508207863,-22.8338748378415,-11.5324793150647));
#10387=CARTESIAN_POINT('Ctrl Pts',(81.3561116693081,-22.6695443672682,-11.5434782667392));
#10388=CARTESIAN_POINT('Ctrl Pts',(81.4038994461849,-22.5129425261447,-11.5544772184136));
#10389=CARTESIAN_POINT('Ctrl Pts',(81.5648482591078,-21.9855089002755,-11.5915215910775));
#10390=CARTESIAN_POINT('Ctrl Pts',(82.0130896610182,-21.5457439380849,-11.6285659637413));
#10391=CARTESIAN_POINT('Ctrl Pts',(82.543499565097,-21.3948927407614,-11.6656103364052));
#10392=CARTESIAN_POINT('Ctrl Pts',(83.0739094691758,-21.2440415434378,-11.702654709069));
#10393=CARTESIAN_POINT('Ctrl Pts',(83.6864878754231,-21.3821041109814,-11.7396990817329));
#10394=CARTESIAN_POINT('Ctrl Pts',(84.1009068497144,-21.7459002954393,-11.7767434543967));
#10395=CARTESIAN_POINT('Ctrl Pts',(84.5153258240058,-22.1096964798972,-11.8137878270606));
#10396=CARTESIAN_POINT('Ctrl Pts',(84.7315853663412,-22.6992262812694,-11.8508321997244));
#10397=CARTESIAN_POINT('Ctrl Pts',(84.6507208542018,-23.2447092606146,-11.8878765723883));
#10398=CARTESIAN_POINT('Ctrl Pts',(84.5698563420624,-23.7901922399597,-11.9249209450521));
#10399=CARTESIAN_POINT('Ctrl Pts',(84.191867775448,-24.2916283972779,-11.961965317716));
#10400=CARTESIAN_POINT('Ctrl Pts',(83.689730161184,-24.5195506788128,-11.9990096903799));
#10401=CARTESIAN_POINT('Ctrl Pts',(83.18759254692,-24.7474729603476,-12.0360540630437));
#10402=CARTESIAN_POINT('Ctrl Pts',(82.5613058850063,-24.7018813660993,-12.0730984357076));
#10403=CARTESIAN_POINT('Ctrl Pts',(82.0974712771361,-24.4036395068296,-12.1101428083714));
#10404=CARTESIAN_POINT('Ctrl Pts',(81.632783413548,-24.1048490111119,-12.147255326711));
#10405=CARTESIAN_POINT('Ctrl Pts',(81.3311467675376,-23.5524778585552,-12.1843678450506));
#10406=CARTESIAN_POINT('Ctrl Pts',(81.3312396675144,-23.0000189535663,-12.2214803633902));
#10407=CARTESIAN_POINT('Ctrl Pts',(81.3341897502355,-23.0015225987737,-12.0285196366098));
#10408=CARTESIAN_POINT('Ctrl Pts',(81.3329525605568,-23.1377669253881,-12.0194092149213));
#10409=CARTESIAN_POINT('Ctrl Pts',(81.3482669854987,-23.2737367791447,-12.0102987932327));
#10410=CARTESIAN_POINT('Ctrl Pts',(81.3812047643192,-23.4052943113693,-12.0011883715442));
#10411=CARTESIAN_POINT('Ctrl Pts',(81.5151348276092,-23.9402274261121,-11.9641439988803));
#10412=CARTESIAN_POINT('Ctrl Pts',(81.9404424442667,-24.4022089641281,-11.9270996262165));
#10413=CARTESIAN_POINT('Ctrl Pts',(82.462498478937,-24.5798270819132,-11.8900552535526));
#10414=CARTESIAN_POINT('Ctrl Pts',(82.9845545136073,-24.7574451996984,-11.8530108808888));
#10415=CARTESIAN_POINT('Ctrl Pts',(83.6033589662905,-24.6506998972526,-11.8159665082249));
#10416=CARTESIAN_POINT('Ctrl Pts',(84.0357347414856,-24.3084399257021,-11.7789221355611));
#10417=CARTESIAN_POINT('Ctrl Pts',(84.4681105166806,-23.9661799541517,-11.7418777628972));
#10418=CARTESIAN_POINT('Ctrl Pts',(84.7140576143876,-23.3884053134966,-11.7048333902334));
#10419=CARTESIAN_POINT('Ctrl Pts',(84.6610258025042,-22.8395170497948,-11.6677890175695));
#10420=CARTESIAN_POINT('Ctrl Pts',(84.6079939906208,-22.290628786093,-11.6307446449057));
#10421=CARTESIAN_POINT('Ctrl Pts',(84.255983269147,-21.7706268993444,-11.5937002722418));
#10422=CARTESIAN_POINT('Ctrl Pts',(83.7660806717326,-21.5174744864626,-11.556655899578));
#10423=CARTESIAN_POINT('Ctrl Pts',(83.2761780743183,-21.2643220735809,-11.5196115269141));
#10424=CARTESIAN_POINT('Ctrl Pts',(82.6483836009633,-21.2780191345659,-11.4825671542502));
#10425=CARTESIAN_POINT('Ctrl Pts',(82.1699883575499,-21.5522976247554,-11.4455227815864));
#10426=CARTESIAN_POINT('Ctrl Pts',(81.6915931141365,-21.826576114945,-11.4084784089225));
#10427=CARTESIAN_POINT('Ctrl Pts',(81.3625971006646,-22.3614360343391,-11.3714340362587));
#10428=CARTESIAN_POINT('Ctrl Pts',(81.3335553674774,-22.9121149578823,-11.3343896635948));
#10429=CARTESIAN_POINT('Ctrl Pts',(81.3320213894825,-22.9412016981782,-11.3324329879332));
#10430=CARTESIAN_POINT('Ctrl Pts',(81.3313242627211,-22.9703325723772,-11.3304763122715));
#10431=CARTESIAN_POINT('Ctrl Pts',(81.3314457178217,-22.9994693778887,-11.3285196366098));
#10432=CARTESIAN_POINT('Origin',(83.,-23.,-12.));
#10433=CARTESIAN_POINT('',(81.3357538816894,-22.9988133680852,-10.6285196366098));
#10434=CARTESIAN_POINT('',(81.3362972869656,-23.0008273571659,-10.8214803633902));
#10435=CARTESIAN_POINT('',(81.334,-23.,-12.));
#10436=CARTESIAN_POINT('Ctrl Pts',(81.3362972869656,-23.0008273571659,-10.8214803633902));
#10437=CARTESIAN_POINT('Ctrl Pts',(81.3377852983276,-22.6697775144948,-10.8435464124149));
#10438=CARTESIAN_POINT('Ctrl Pts',(81.4333699328181,-22.3379359375284,-10.8656124614396));
#10439=CARTESIAN_POINT('Ctrl Pts',(81.6172641946395,-22.0657603876407,-10.8876785104643));
#10440=CARTESIAN_POINT('Ctrl Pts',(81.9259849610095,-21.6088334367057,-10.9247228831281));
#10441=CARTESIAN_POINT('Ctrl Pts',(82.4835933983085,-21.3200663904382,-10.961767255792));
#10442=CARTESIAN_POINT('Ctrl Pts',(83.0349169120014,-21.3316047320903,-10.9988116284558));
#10443=CARTESIAN_POINT('Ctrl Pts',(83.5862404256943,-21.3431430737424,-11.0358560011197));
#10444=CARTESIAN_POINT('Ctrl Pts',(84.1312790157812,-21.6549868033142,-11.0729003737835));
#10445=CARTESIAN_POINT('Ctrl Pts',(84.4206122971833,-22.1244300931287,-11.1099447464474));
#10446=CARTESIAN_POINT('Ctrl Pts',(84.7099455785855,-22.5938733829432,-11.1469891191112));
#10447=CARTESIAN_POINT('Ctrl Pts',(84.7435735513029,-23.2209162330006,-11.1840334917751));
#10448=CARTESIAN_POINT('Ctrl Pts',(84.506107393228,-23.7186114950314,-11.2210778644389));
#10449=CARTESIAN_POINT('Ctrl Pts',(84.2686412351531,-24.2163067570623,-11.2581222371028));
#10450=CARTESIAN_POINT('Ctrl Pts',(83.7600809462859,-24.5846544310667,-11.2951666097666));
#10451=CARTESIAN_POINT('Ctrl Pts',(83.213153723181,-24.6550913724086,-11.3322109824305));
#10452=CARTESIAN_POINT('Ctrl Pts',(82.6662265000761,-24.7255283137505,-11.3692553550943));
#10453=CARTESIAN_POINT('Ctrl Pts',(82.0809323427335,-24.4980545224299,-11.4062997277582));
#10454=CARTESIAN_POINT('Ctrl Pts',(81.72511337603,-24.0767664819958,-11.4433441004221));
#10455=CARTESIAN_POINT('Ctrl Pts',(81.4749416463615,-23.7805642903574,-11.4693895214114));
#10456=CARTESIAN_POINT('Ctrl Pts',(81.3382067289016,-23.3885536127611,-11.4954349424008));
#10457=CARTESIAN_POINT('Ctrl Pts',(81.3350035286226,-22.9985661148555,-11.5214803633902));
#10458=CARTESIAN_POINT('Ctrl Pts',(81.3314457178217,-22.9994693778887,-11.3285196366098));
#10459=CARTESIAN_POINT('Ctrl Pts',(81.3336236872483,-23.5219593456538,-11.2934319396076));
#10460=CARTESIAN_POINT('Ctrl Pts',(81.5990309145572,-24.0463566302869,-11.2583442426054));
#10461=CARTESIAN_POINT('Ctrl Pts',(82.0223180957112,-24.3523681406768,-11.2232565456033));
#10462=CARTESIAN_POINT('Ctrl Pts',(82.4692100100346,-24.6754444722357,-11.1862121729394));
#10463=CARTESIAN_POINT('Ctrl Pts',(83.092081291584,-24.7550992076612,-11.1491678002756));
#10464=CARTESIAN_POINT('Ctrl Pts',(83.6058937839349,-24.5548807724326,-11.1121234276117));
#10465=CARTESIAN_POINT('Ctrl Pts',(84.1197062762858,-24.354662337204,-11.0750790549479));
#10466=CARTESIAN_POINT('Ctrl Pts',(84.5244599794382,-23.8745707313213,-11.038034682284));
#10467=CARTESIAN_POINT('Ctrl Pts',(84.6349316333544,-23.3343053217472,-11.0009903096202));
#10468=CARTESIAN_POINT('Ctrl Pts',(84.7454032872706,-22.7940399121731,-10.9639459369563));
#10469=CARTESIAN_POINT('Ctrl Pts',(84.5615928919505,-22.1936006989076,-10.9269015642925));
#10470=CARTESIAN_POINT('Ctrl Pts',(84.167615701646,-21.8077604824695,-10.8898571916286));
#10471=CARTESIAN_POINT('Ctrl Pts',(83.7736385113415,-21.4219202660315,-10.8528128189647));
#10472=CARTESIAN_POINT('Ctrl Pts',(83.1694945260525,-21.2506790464209,-10.8157684463009));
#10473=CARTESIAN_POINT('Ctrl Pts',(82.631651922885,-21.3724001757259,-10.778724073637));
#10474=CARTESIAN_POINT('Ctrl Pts',(82.0938093197176,-21.4941213050309,-10.7416797009732));
#10475=CARTESIAN_POINT('Ctrl Pts',(81.6222680986716,-21.9088047832515,-10.7046353283093));
#10476=CARTESIAN_POINT('Ctrl Pts',(81.4328148023386,-22.4266832898627,-10.6675909556455));
#10477=CARTESIAN_POINT('Ctrl Pts',(81.3662082829035,-22.6087549955722,-10.6545671826336));
#10478=CARTESIAN_POINT('Ctrl Pts',(81.3344686881453,-22.80358192037,-10.6415434096217));
#10479=CARTESIAN_POINT('Ctrl Pts',(81.3357538816894,-22.9988133680852,-10.6285196366098));
#10480=CARTESIAN_POINT('Origin',(83.,-23.,-12.));
#10481=CARTESIAN_POINT('',(81.3357307175978,-23.0011975492408,-9.92851963660979));
#10482=CARTESIAN_POINT('',(81.3319839174274,-23.0009873429913,-10.1214803633902));
#10483=CARTESIAN_POINT('',(81.334,-23.,-12.));
#10484=CARTESIAN_POINT('Ctrl Pts',(81.3319839174274,-23.0009873429913,-10.1214803633902));
#10485=CARTESIAN_POINT('Ctrl Pts',(81.3354512767123,-22.5071811287366,-10.1546135097651));
#10486=CARTESIAN_POINT('Ctrl Pts',(81.5685740227169,-22.0105308872886,-10.18774665614));
#10487=CARTESIAN_POINT('Ctrl Pts',(81.9525268434233,-21.700938051139,-10.2208798025149));
#10488=CARTESIAN_POINT('Ctrl Pts',(82.3818036532575,-21.3547991041577,-10.2579241751788));
#10489=CARTESIAN_POINT('Ctrl Pts',(82.9996220147682,-21.242486822828,-10.2949685478426));
#10490=CARTESIAN_POINT('Ctrl Pts',(83.523256087181,-21.4153975173706,-10.3320129205065));
#10491=CARTESIAN_POINT('Ctrl Pts',(84.0468901595938,-21.5883082119132,-10.3690572931703));
#10492=CARTESIAN_POINT('Ctrl Pts',(84.4763399429088,-22.0464418823281,-10.4061016658342));
#10493=CARTESIAN_POINT('Ctrl Pts',(84.6150807647917,-22.5801475450506,-10.443146038498));
#10494=CARTESIAN_POINT('Ctrl Pts',(84.7538215866746,-23.1138532077731,-10.4801904111619));
#10495=CARTESIAN_POINT('Ctrl Pts',(84.6018534471254,-23.7231308628033,-10.5172347838257));
#10496=CARTESIAN_POINT('Ctrl Pts',(84.2287199575057,-24.1291630647319,-10.5542791564896));
#10497=CARTESIAN_POINT('Ctrl Pts',(83.8555864678859,-24.5351952666605,-10.5913235291534));
#10498=CARTESIAN_POINT('Ctrl Pts',(83.2612876281956,-24.7379820154875,-10.6283679018173));
#10499=CARTESIAN_POINT('Ctrl Pts',(82.7177862831642,-24.6447241041454,-10.6654122744811));
#10500=CARTESIAN_POINT('Ctrl Pts',(82.1742849381328,-24.5514661928033,-10.702456647145));
#10501=CARTESIAN_POINT('Ctrl Pts',(81.6815810877603,-24.1621636212921,-10.7395010198088));
#10502=CARTESIAN_POINT('Ctrl Pts',(81.4651457102945,-23.6549689077352,-10.7765453924727));
#10503=CARTESIAN_POINT('Ctrl Pts',(81.3776333866262,-23.4498925082327,-10.7915237161119));
#10504=CARTESIAN_POINT('Ctrl Pts',(81.3352872323004,-23.2255423334935,-10.806502039751));
#10505=CARTESIAN_POINT('Ctrl Pts',(81.3362972869656,-23.0008273571659,-10.8214803633902));
#10506=CARTESIAN_POINT('Ctrl Pts',(81.3357538816894,-22.9988133680852,-10.6285196366098));
#10507=CARTESIAN_POINT('Ctrl Pts',(81.3381242485233,-23.3588915451814,-10.6044990369578));
#10508=CARTESIAN_POINT('Ctrl Pts',(81.4528345315299,-23.720345781685,-10.5804784373059));
#10509=CARTESIAN_POINT('Ctrl Pts',(81.6683272585003,-24.005688422643,-10.5564578376539));
#10510=CARTESIAN_POINT('Ctrl Pts',(82.0006583826149,-24.4457415138104,-10.5194134649901));
#10511=CARTESIAN_POINT('Ctrl Pts',(82.5726860024639,-24.7047741611435,-10.4823690923262));
#10512=CARTESIAN_POINT('Ctrl Pts',(83.1226390218108,-24.6642479275098,-10.4453247196624));
#10513=CARTESIAN_POINT('Ctrl Pts',(83.6725920411577,-24.6237216938762,-10.4082803469985));
#10514=CARTESIAN_POINT('Ctrl Pts',(84.2004704600023,-24.2836365792757,-10.3712359743347));
#10515=CARTESIAN_POINT('Ctrl Pts',(84.4647067253352,-23.7996222249595,-10.3341916016708));
#10516=CARTESIAN_POINT('Ctrl Pts',(84.7289429906682,-23.3156078706434,-10.297147229007));
#10517=CARTESIAN_POINT('Ctrl Pts',(84.7295371024896,-22.6876642766114,-10.2601028563431));
#10518=CARTESIAN_POINT('Ctrl Pts',(84.4662171835379,-22.2031507893022,-10.2230584836792));
#10519=CARTESIAN_POINT('Ctrl Pts',(84.2028972645862,-21.718637301993,-10.1860141110154));
#10520=CARTESIAN_POINT('Ctrl Pts',(83.6756633148615,-21.3775539214065,-10.1489697383515));
#10521=CARTESIAN_POINT('Ctrl Pts',(83.1257879656207,-21.3359871149548,-10.1119253656877));
#10522=CARTESIAN_POINT('Ctrl Pts',(82.57591261638,-21.294420308503,-10.0748809930238));
#10523=CARTESIAN_POINT('Ctrl Pts',(82.0033958676232,-21.5523700761859,-10.03783662036));
#10524=CARTESIAN_POINT('Ctrl Pts',(81.6702326506014,-21.9917935279097,-10.0007922476961));
#10525=CARTESIAN_POINT('Ctrl Pts',(81.4535683830342,-22.2775614502231,-9.97670137733401));
#10526=CARTESIAN_POINT('Ctrl Pts',(81.3381320398903,-22.6400786239042,-9.9526105069719));
#10527=CARTESIAN_POINT('Ctrl Pts',(81.3357307175978,-23.0011975492408,-9.92851963660979));
#10528=CARTESIAN_POINT('Origin',(83.,-23.,-12.));
#10529=CARTESIAN_POINT('',(81.331431843514,-23.0005124578661,-9.22851963660979));
#10530=CARTESIAN_POINT('',(81.3333049370251,-22.9985455594153,-9.42148036339021));
#10531=CARTESIAN_POINT('',(81.334,-23.,-12.));
#10532=CARTESIAN_POINT('Ctrl Pts',(81.3333049370251,-22.9985455594153,-9.42148036339021));
#10533=CARTESIAN_POINT('Ctrl Pts',(81.3323267498425,-22.8916766658214,-9.42863623445147));
#10534=CARTESIAN_POINT('Ctrl Pts',(81.3417252765875,-22.7849791349272,-9.43579210551273));
#10535=CARTESIAN_POINT('Ctrl Pts',(81.3621246357665,-22.6804280175552,-9.44294797657399));
#10536=CARTESIAN_POINT('Ctrl Pts',(81.4677276374222,-22.1391898480586,-9.47999234923785));
#10537=CARTESIAN_POINT('Ctrl Pts',(81.8681425497088,-21.655473532047,-9.5170367219017));
#10538=CARTESIAN_POINT('Ctrl Pts',(82.3801316286753,-21.4506371751721,-9.55408109456555));
#10539=CARTESIAN_POINT('Ctrl Pts',(82.8921207076418,-21.2458008182972,-9.59112546722941));
#10540=CARTESIAN_POINT('Ctrl Pts',(83.5156839532884,-21.3198444205589,-9.62816983989325));
#10541=CARTESIAN_POINT('Ctrl Pts',(83.965466552802,-21.6388841723983,-9.66521421255711));
#10542=CARTESIAN_POINT('Ctrl Pts',(84.4152491523155,-21.9579239242376,-9.70225858522096));
#10543=CARTESIAN_POINT('Ctrl Pts',(84.6912511056959,-22.5219598256545,-9.73930295788482));
#10544=CARTESIAN_POINT('Ctrl Pts',(84.667168487411,-23.0728779480423,-9.77634733054867));
#10545=CARTESIAN_POINT('Ctrl Pts',(84.6430858691261,-23.6237960704302,-9.81339170321253));
#10546=CARTESIAN_POINT('Ctrl Pts',(84.3189186791757,-24.161596413789,-9.85043607587638));
#10547=CARTESIAN_POINT('Ctrl Pts',(83.8430122032293,-24.44017095719,-9.88748044854023));
#10548=CARTESIAN_POINT('Ctrl Pts',(83.3671057272829,-24.7187455005911,-9.92452482120408));
#10549=CARTESIAN_POINT('Ctrl Pts',(82.7394599653405,-24.7380942440345,-9.96156919386794));
#10550=CARTESIAN_POINT('Ctrl Pts',(82.2472979700152,-24.4893628217409,-9.99861356653179));
#10551=CARTESIAN_POINT('Ctrl Pts',(81.7551359746898,-24.2406313994473,-10.0356579391956));
#10552=CARTESIAN_POINT('Ctrl Pts',(81.3984577459816,-23.7238198114168,-10.0727023118595));
#10553=CARTESIAN_POINT('Ctrl Pts',(81.3404862607064,-23.175431211085,-10.1097466845233));
#10554=CARTESIAN_POINT('Ctrl Pts',(81.3343655038704,-23.1175311373102,-10.1136579108123));
#10555=CARTESIAN_POINT('Ctrl Pts',(81.3315746104864,-23.0592790556162,-10.1175691371013));
#10556=CARTESIAN_POINT('Ctrl Pts',(81.3319839174274,-23.0009873429913,-10.1214803633902));
#10557=CARTESIAN_POINT('Ctrl Pts',(81.3357307175978,-23.0011975492408,-9.92851963660979));
#10558=CARTESIAN_POINT('Ctrl Pts',(81.3344395424192,-23.1953688166229,-9.91556613430805));
#10559=CARTESIAN_POINT('Ctrl Pts',(81.3658283975604,-23.3891358305449,-9.90261263200631));
#10560=CARTESIAN_POINT('Ctrl Pts',(81.4317327528845,-23.5703501867417,-9.88965912970457));
#10561=CARTESIAN_POINT('Ctrl Pts',(81.6202057574764,-24.088586258085,-9.85261475704071));
#10562=CARTESIAN_POINT('Ctrl Pts',(82.0909614519471,-24.5041612650069,-9.81557038437686));
#10563=CARTESIAN_POINT('Ctrl Pts',(82.6285727661251,-24.6268999059032,-9.77852601171301));
#10564=CARTESIAN_POINT('Ctrl Pts',(83.1661840803031,-24.7496385467995,-9.74148163904916));
#10565=CARTESIAN_POINT('Ctrl Pts',(83.7706510141882,-24.5795408216701,-9.7044372663853));
#10566=CARTESIAN_POINT('Ctrl Pts',(84.1653576030415,-24.1944467970255,-9.66739289372145));
#10567=CARTESIAN_POINT('Ctrl Pts',(84.5600641918947,-23.8093527723809,-9.63034852105759));
#10568=CARTESIAN_POINT('Ctrl Pts',(84.745010435716,-23.2092624482211,-9.59330414839375));
#10569=CARTESIAN_POINT('Ctrl Pts',(84.635561293626,-22.6687889665429,-9.55625977572989));
#10570=CARTESIAN_POINT('Ctrl Pts',(84.5261121515361,-22.1283154848647,-9.51921540306604));
#10571=CARTESIAN_POINT('Ctrl Pts',(84.1222676235349,-21.6474588456682,-9.48217103040219));
#10572=CARTESIAN_POINT('Ctrl Pts',(83.6088349132188,-21.4462685102183,-9.44512665773833));
#10573=CARTESIAN_POINT('Ctrl Pts',(83.0954022029027,-21.2450781747684,-9.40808228507448));
#10574=CARTESIAN_POINT('Ctrl Pts',(82.4723813102717,-21.3235541430652,-9.37103791241062));
#10575=CARTESIAN_POINT('Ctrl Pts',(82.0248788567251,-21.6457842676196,-9.33399353974677));
#10576=CARTESIAN_POINT('Ctrl Pts',(81.600164502517,-21.9516055165803,-9.29883557203444));
#10577=CARTESIAN_POINT('Ctrl Pts',(81.3335479331276,-22.4769876979749,-9.26367760432212));
#10578=CARTESIAN_POINT('Ctrl Pts',(81.331431843514,-23.0005124578661,-9.22851963660979));
#10579=CARTESIAN_POINT('Origin',(83.,-23.,-12.));
#10580=CARTESIAN_POINT('',(81.3342212297538,-22.9984780339595,-8.52851963660979));
#10581=CARTESIAN_POINT('',(81.3367006367545,-22.9999263102539,-8.72148036339021));
#10582=CARTESIAN_POINT('',(81.334,-23.,-12.));
#10583=CARTESIAN_POINT('Ctrl Pts',(81.3367006367545,-22.9999263102539,-8.72148036339021));
#10584=CARTESIAN_POINT('Ctrl Pts',(81.3365926969101,-22.7263673067472,-8.73970333180169));
#10585=CARTESIAN_POINT('Ctrl Pts',(81.4003183665741,-22.4528556568932,-8.75792630021316));
#10586=CARTESIAN_POINT('Ctrl Pts',(81.5281532603125,-22.2135973451411,-8.77614926862464));
#10587=CARTESIAN_POINT('Ctrl Pts',(81.7880211005105,-21.7272235632556,-8.81319364128849));
#10588=CARTESIAN_POINT('Ctrl Pts',(82.3128162721351,-21.3823995440889,-8.85023801395235));
#10589=CARTESIAN_POINT('Ctrl Pts',(82.8623821768039,-21.3369235449087,-8.8872823866162));
#10590=CARTESIAN_POINT('Ctrl Pts',(83.4119480814727,-21.2914475457284,-8.92432675928005));
#10591=CARTESIAN_POINT('Ctrl Pts',(83.9862847191857,-21.5453195665347,-8.9613711319439));
#10592=CARTESIAN_POINT('Ctrl Pts',(84.3225643416799,-21.9823627744406,-8.99841550460776));
#10593=CARTESIAN_POINT('Ctrl Pts',(84.658843964174,-22.4194059823464,-9.03545987727161));
#10594=CARTESIAN_POINT('Ctrl Pts',(84.7570665714493,-23.0396203773518,-9.07250424993546));
#10595=CARTESIAN_POINT('Ctrl Pts',(84.5722835654198,-23.5591836466087,-9.10954862259931));
#10596=CARTESIAN_POINT('Ctrl Pts',(84.3875005593903,-24.0787469158655,-9.14659299526317));
#10597=CARTESIAN_POINT('Ctrl Pts',(83.9197119400561,-24.4976590593737,-9.18363736792702));
#10598=CARTESIAN_POINT('Ctrl Pts',(83.3829869856121,-24.62421763615,-9.22068174059087));
#10599=CARTESIAN_POINT('Ctrl Pts',(82.8462620311681,-24.7507762129263,-9.25772611325472));
#10600=CARTESIAN_POINT('Ctrl Pts',(82.2406007416144,-24.5849812229706,-9.29477048591858));
#10601=CARTESIAN_POINT('Ctrl Pts',(81.84316564235,-24.202703716502,-9.33181485858243));
#10602=CARTESIAN_POINT('Ctrl Pts',(81.5225031841386,-23.8942708549605,-9.36170336018503));
#10603=CARTESIAN_POINT('Ctrl Pts',(81.3373906100235,-23.4449134537085,-9.39159186178762));
#10604=CARTESIAN_POINT('Ctrl Pts',(81.3333049370251,-22.9985455594153,-9.42148036339021));
#10605=CARTESIAN_POINT('Ctrl Pts',(81.331431843514,-23.0005124578661,-9.22851963660979));
#10606=CARTESIAN_POINT('Ctrl Pts',(81.3313183044734,-23.0286022413082,-9.22663323165827));
#10607=CARTESIAN_POINT('Ctrl Pts',(81.3319662284119,-23.056686677472,-9.22474682670674));
#10608=CARTESIAN_POINT('Ctrl Pts',(81.3333920509507,-23.084731564703,-9.22286042175522));
#10609=CARTESIAN_POINT('Ctrl Pts',(81.3613917131847,-23.6354644564197,-9.18581604909136));
#10610=CARTESIAN_POINT('Ctrl Pts',(81.6893750521149,-24.170945959041,-9.1487716764275));
#10611=CARTESIAN_POINT('Ctrl Pts',(82.1672504371963,-24.4461291987769,-9.11172730376365));
#10612=CARTESIAN_POINT('Ctrl Pts',(82.6451258222777,-24.7213124385128,-9.0746829310998));
#10613=CARTESIAN_POINT('Ctrl Pts',(83.2728932535105,-24.7361974153634,-9.03763855843595));
#10614=CARTESIAN_POINT('Ctrl Pts',(83.7632740000222,-24.4839724710224,-9.0005941857721));
#10615=CARTESIAN_POINT('Ctrl Pts',(84.2536547465338,-24.2317475266814,-8.96354981310824));
#10616=CARTESIAN_POINT('Ctrl Pts',(84.6066488083243,-23.7124126611489,-8.92650544044439));
#10617=CARTESIAN_POINT('Ctrl Pts',(84.6607191558582,-23.1636257292351,-8.88946106778053));
#10618=CARTESIAN_POINT('Ctrl Pts',(84.7147895033921,-22.6148387973213,-8.85241669511668));
#10619=CARTESIAN_POINT('Ctrl Pts',(84.4699361366694,-22.0365997990262,-8.81537232245283));
#10620=CARTESIAN_POINT('Ctrl Pts',(84.0382087749791,-21.6935222797378,-8.77832794978898));
#10621=CARTESIAN_POINT('Ctrl Pts',(83.6064814132889,-21.3504447604494,-8.74128357712513));
#10622=CARTESIAN_POINT('Ctrl Pts',(82.9878800566311,-21.2425287201677,-8.70423920446127));
#10623=CARTESIAN_POINT('Ctrl Pts',(82.4654888597494,-21.4191586624222,-8.66719483179742));
#10624=CARTESIAN_POINT('Ctrl Pts',(81.9430976628678,-21.5957886046768,-8.63015045913356));
#10625=CARTESIAN_POINT('Ctrl Pts',(81.5169166257624,-22.0569645294676,-8.59310608646971));
#10626=CARTESIAN_POINT('Ctrl Pts',(81.3819745782115,-22.5916432582957,-8.55606171380586));
#10627=CARTESIAN_POINT('Ctrl Pts',(81.3485319433084,-22.7241524786849,-8.54688102140717));
#10628=CARTESIAN_POINT('Ctrl Pts',(81.3329770659435,-22.861176205662,-8.53770032900848));
#10629=CARTESIAN_POINT('Ctrl Pts',(81.3342212297538,-22.9984780339595,-8.52851963660979));
#10630=CARTESIAN_POINT('Origin',(83.,-23.,-12.));
#10631=CARTESIAN_POINT('',(81.3366058837444,-23.0004198226253,-7.82851963660979));
#10632=CARTESIAN_POINT('',(81.3335753931735,-23.0014929636922,-8.02148036339021));
#10633=CARTESIAN_POINT('',(81.334,-23.,-12.));
#10634=CARTESIAN_POINT('Ctrl Pts',(81.3335753931735,-23.0014929636922,-8.02148036339021));
#10635=CARTESIAN_POINT('Ctrl Pts',(81.337614240534,-22.5638796924227,-8.05077042915191));
#10636=CARTESIAN_POINT('Ctrl Pts',(81.5146048346072,-22.123375374204,-8.0800604949136));
#10637=CARTESIAN_POINT('Ctrl Pts',(81.8239355420513,-21.8160936061122,-8.10935056067529));
#10638=CARTESIAN_POINT('Ctrl Pts',(82.2151590406997,-21.4274614868599,-8.14639493333914));
#10639=CARTESIAN_POINT('Ctrl Pts',(82.8180700802442,-21.2519284296373,-8.18343930600298));
#10640=CARTESIAN_POINT('Ctrl Pts',(83.356764705155,-21.3698218175571,-8.22048367866684));
#10641=CARTESIAN_POINT('Ctrl Pts',(83.8954593300658,-21.4877152054768,-8.25752805133069));
#10642=CARTESIAN_POINT('Ctrl Pts',(84.369937540343,-21.8990350385389,-8.29457242399455));
#10643=CARTESIAN_POINT('Ctrl Pts',(84.5630687686518,-22.415553265601,-8.33161679665841));
#10644=CARTESIAN_POINT('Ctrl Pts',(84.7561999969607,-22.9320714926631,-8.36866116932226));
#10645=CARTESIAN_POINT('Ctrl Pts',(84.6679842433012,-23.5537881137252,-8.40570554198611));
#10646=CARTESIAN_POINT('Ctrl Pts',(84.3387907729539,-23.9961933681454,-8.44274991464996));
#10647=CARTESIAN_POINT('Ctrl Pts',(84.0095973026066,-24.4385986225656,-8.47979428731381));
#10648=CARTESIAN_POINT('Ctrl Pts',(83.4394261155714,-24.701692510344,-8.51683865997767));
#10649=CARTESIAN_POINT('Ctrl Pts',(82.8891987677264,-24.6650780905852,-8.55388303264152));
#10650=CARTESIAN_POINT('Ctrl Pts',(82.3389714198814,-24.6284636708265,-8.59092740530537));
#10651=CARTESIAN_POINT('Ctrl Pts',(81.8086879112266,-24.2921409435307,-8.62797177796922));
#10652=CARTESIAN_POINT('Ctrl Pts',(81.5410164112849,-23.8100178075807,-8.66501615063307));
#10653=CARTESIAN_POINT('Ctrl Pts',(81.4050186025769,-23.5650619940897,-8.68383755488545));
#10654=CARTESIAN_POINT('Ctrl Pts',(81.3368121213051,-23.2824688947341,-8.70265895913783));
#10655=CARTESIAN_POINT('Ctrl Pts',(81.3367006367545,-22.9999263102539,-8.72148036339021));
#10656=CARTESIAN_POINT('Ctrl Pts',(81.3342212297538,-22.9984780339595,-8.52851963660979));
#10657=CARTESIAN_POINT('Ctrl Pts',(81.3379973047056,-23.4151932529611,-8.50065595634463));
#10658=CARTESIAN_POINT('Ctrl Pts',(81.4965162247509,-23.8344701770685,-8.47279227607947));
#10659=CARTESIAN_POINT('Ctrl Pts',(81.7793408475925,-24.1378720174819,-8.4449285958143));
#10660=CARTESIAN_POINT('Ctrl Pts',(82.1553522225205,-24.5412405149744,-8.40788422315045));
#10661=CARTESIAN_POINT('Ctrl Pts',(82.7510780303727,-24.7397959770939,-8.37083985048659));
#10662=CARTESIAN_POINT('Ctrl Pts',(83.293902417857,-24.6426755189852,-8.33379547782274));
#10663=CARTESIAN_POINT('Ctrl Pts',(83.8367268053414,-24.5455550608765,-8.29675110515889));
#10664=CARTESIAN_POINT('Ctrl Pts',(84.326649772458,-24.1527586825395,-8.25970673249504));
#10665=CARTESIAN_POINT('Ctrl Pts',(84.5394729275635,-23.6440377325831,-8.22266235983118));
#10666=CARTESIAN_POINT('Ctrl Pts',(84.7522960826691,-23.1353167826267,-8.18561798716733));
#10667=CARTESIAN_POINT('Ctrl Pts',(84.6880194257635,-22.5106712610509,-8.14857361450348));
#10668=CARTESIAN_POINT('Ctrl Pts',(84.3760572205986,-22.055951259959,-8.11152924183962));
#10669=CARTESIAN_POINT('Ctrl Pts',(84.0640950154338,-21.601231258867,-8.07448486917577));
#10670=CARTESIAN_POINT('Ctrl Pts',(83.5044472620097,-21.3164367782588,-8.03744049651192));
#10671=CARTESIAN_POINT('Ctrl Pts',(82.9532197848582,-21.3318953601593,-8.00039612384806));
#10672=CARTESIAN_POINT('Ctrl Pts',(82.4019923077066,-21.3473539420599,-7.96335175118421));
#10673=CARTESIAN_POINT('Ctrl Pts',(81.8591851068275,-21.6630655864691,-7.92630737852036));
#10674=CARTESIAN_POINT('Ctrl Pts',(81.5731974420689,-22.1345544656655,-7.8892630058565));
#10675=CARTESIAN_POINT('Ctrl Pts',(81.416881713379,-22.3922618314115,-7.8690152161076));
#10676=CARTESIAN_POINT('Ctrl Pts',(81.3372913231897,-22.6965079505961,-7.84876742635869));
#10677=CARTESIAN_POINT('Ctrl Pts',(81.3366058837444,-23.0004198226253,-7.82851963660979));
#10678=CARTESIAN_POINT('Origin',(83.,-23.,-12.));
#10679=CARTESIAN_POINT('',(81.3326823670782,-23.0013023207031,-7.12851963660979));
#10680=CARTESIAN_POINT('',(81.3317907907837,-22.9991411291167,-7.32148036339021));
#10681=CARTESIAN_POINT('',(81.334,-23.,-12.));
#10682=CARTESIAN_POINT('Ctrl Pts',(81.3317907907837,-22.9991411291167,-7.32148036339021));
#10683=CARTESIAN_POINT('Ctrl Pts',(81.3314807411988,-22.9497833657722,-7.32479315383826));
#10684=CARTESIAN_POINT('Ctrl Pts',(81.3334814629917,-22.9004510906902,-7.32810594428632));
#10685=CARTESIAN_POINT('Ctrl Pts',(81.337874792749,-22.851332821333,-7.33141873473437));
#10686=CARTESIAN_POINT('Ctrl Pts',(81.3870020005563,-22.302081215111,-7.36846310739822));
#10687=CARTESIAN_POINT('Ctrl Pts',(81.7353061391843,-21.7795893526127,-7.40550748006207));
#10688=CARTESIAN_POINT('Ctrl Pts',(82.223396212068,-21.5229595829052,-7.44255185272593));
#10689=CARTESIAN_POINT('Ctrl Pts',(82.7114862849517,-21.2663298131978,-7.47959622538978));
#10690=CARTESIAN_POINT('Ctrl Pts',(83.339362292091,-21.2755621362812,-7.51664059805363));
#10691=CARTESIAN_POINT('Ctrl Pts',(83.8196959004573,-21.5464317645881,-7.55368497071749));
#10692=CARTESIAN_POINT('Ctrl Pts',(84.3000295088237,-21.8173013928951,-7.59072934338134));
#10693=CARTESIAN_POINT('Ctrl Pts',(84.6328207184171,-22.3498083264256,-7.62777371604519));
#10694=CARTESIAN_POINT('Ctrl Pts',(84.6657776801849,-22.9002668600333,-7.66481808870904));
#10695=CARTESIAN_POINT('Ctrl Pts',(84.6987346419527,-23.450725393641,-7.7018624613729));
#10696=CARTESIAN_POINT('Ctrl Pts',(84.4318573558949,-24.0191355273259,-7.73890683403675));
#10697=CARTESIAN_POINT('Ctrl Pts',(83.9872741414016,-24.3453816241485,-7.77595120670061));
#10698=CARTESIAN_POINT('Ctrl Pts',(83.5426909269083,-24.6716277209712,-7.81299557936446));
#10699=CARTESIAN_POINT('Ctrl Pts',(82.9204017839794,-24.7557097809315,-7.85003995202831));
#10700=CARTESIAN_POINT('Ctrl Pts',(82.4051784603229,-24.5591501854178,-7.88708432469216));
#10701=CARTESIAN_POINT('Ctrl Pts',(81.8899551366663,-24.362590589904,-7.92412869735602));
#10702=CARTESIAN_POINT('Ctrl Pts',(81.4817976322821,-23.8853893389161,-7.96117307001987));
#10703=CARTESIAN_POINT('Ctrl Pts',(81.3674868589662,-23.3459231227812,-7.99821744268372));
#10704=CARTESIAN_POINT('Ctrl Pts',(81.3435587761084,-23.2329994503731,-8.00597174958589));
#10705=CARTESIAN_POINT('Ctrl Pts',(81.332506141154,-23.1173475212576,-8.01372605648805));
#10706=CARTESIAN_POINT('Ctrl Pts',(81.3335753931735,-23.0014929636922,-8.02148036339021));
#10707=CARTESIAN_POINT('Ctrl Pts',(81.3366058837444,-23.0004198226253,-7.82851963660979));
#10708=CARTESIAN_POINT('Ctrl Pts',(81.3360372764733,-23.2525303502769,-7.81172305369484));
#10709=CARTESIAN_POINT('Ctrl Pts',(81.3897675507874,-23.5044108638859,-7.79492647077989));
#10710=CARTESIAN_POINT('Ctrl Pts',(81.4990409610885,-23.7293034217695,-7.77812988786494));
#10711=CARTESIAN_POINT('Ctrl Pts',(81.7400402735046,-24.2252973846937,-7.74108551520109));
#10712=CARTESIAN_POINT('Ctrl Pts',(82.2512070269747,-24.5900191965585,-7.70404114253724));
#10713=CARTESIAN_POINT('Ctrl Pts',(82.7986212649283,-24.6565651134249,-7.66699676987338));
#10714=CARTESIAN_POINT('Ctrl Pts',(83.3460355028819,-24.7231110302912,-7.62995239720953));
#10715=CARTESIAN_POINT('Ctrl Pts',(83.929697225319,-24.4914810521591,-7.59290802454568));
#10716=CARTESIAN_POINT('Ctrl Pts',(84.282511322795,-24.067673346594,-7.55586365188182));
#10717=CARTESIAN_POINT('Ctrl Pts',(84.635325420271,-23.6438656410289,-7.51881927921797));
#10718=CARTESIAN_POINT('Ctrl Pts',(84.7572918927858,-23.0278802080309,-7.48177490655412));
#10719=CARTESIAN_POINT('Ctrl Pts',(84.5925965199425,-22.5016046403627,-7.44473053389027));
#10720=CARTESIAN_POINT('Ctrl Pts',(84.4279011470992,-21.9753290726945,-7.40768616122642));
#10721=CARTESIAN_POINT('Ctrl Pts',(83.9765439288979,-21.5387633703561,-7.37064178856256));
#10722=CARTESIAN_POINT('Ctrl Pts',(83.4450747358265,-21.3916875211121,-7.33359741589871));
#10723=CARTESIAN_POINT('Ctrl Pts',(82.9136055427551,-21.2446116718681,-7.29655304323486));
#10724=CARTESIAN_POINT('Ctrl Pts',(82.3020243748137,-21.3870256757184,-7.259508670571));
#10725=CARTESIAN_POINT('Ctrl Pts',(81.8902029601806,-21.7537602138678,-7.22246429790715));
#10726=CARTESIAN_POINT('Ctrl Pts',(81.5420761010417,-22.0637735797765,-7.19114941080803));
#10727=CARTESIAN_POINT('Ctrl Pts',(81.3366956550969,-22.5340842585654,-7.15983452370891));
#10728=CARTESIAN_POINT('Ctrl Pts',(81.3326823670782,-23.0013023207031,-7.12851963660979));
#10729=CARTESIAN_POINT('Origin',(83.,-23.,-12.));
#10730=CARTESIAN_POINT('',(81.3325225746862,-22.9987867636662,-6.42851963660979));
#10731=CARTESIAN_POINT('',(81.3361555725406,-22.9990558295284,-6.62148036339021));
#10732=CARTESIAN_POINT('',(81.334,-23.,-12.));
#10733=CARTESIAN_POINT('',(84.2690708798524,-21.9206413469515,-6.));
#10734=CARTESIAN_POINT('Ctrl Pts',(81.3325225746862,-22.9987867636662,-6.42851963660979));
#10735=CARTESIAN_POINT('Ctrl Pts',(81.3364572466955,-23.4716253593496,-6.39681287573142));
#10736=CARTESIAN_POINT('Ctrl Pts',(81.547620038085,-23.9474489563196,-6.36510611485305));
#10737=CARTESIAN_POINT('Ctrl Pts',(81.903404325475,-24.2577326133438,-6.33339935397467));
#10738=CARTESIAN_POINT('Ctrl Pts',(82.3190824132044,-24.6202503573164,-6.29635498131082));
#10739=CARTESIAN_POINT('Ctrl Pts',(82.9321725171365,-24.7568018776601,-6.25931060864697));
#10740=CARTESIAN_POINT('Ctrl Pts',(83.462047088432,-24.6038092974618,-6.22226623598312));
#10741=CARTESIAN_POINT('Ctrl Pts',(83.9919216597275,-24.4508167172636,-6.18522186331926));
#10742=CARTESIAN_POINT('Ctrl Pts',(84.4385806983865,-24.0082800365234,-6.14817749065541));
#10743=CARTESIAN_POINT('Ctrl Pts',(84.5975922580266,-23.4812307285184,-6.11113311799156));
#10744=CARTESIAN_POINT('Ctrl Pts',(84.7566038176667,-22.9541814205133,-6.0740887453277));
#10745=CARTESIAN_POINT('Ctrl Pts',(84.627967898288,-22.3426194852432,-6.03704437266385));
#10746=CARTESIAN_POINT('Ctrl Pts',(84.2690708798524,-21.9206413469515,-6.));
#10747=CARTESIAN_POINT('',(81.7285275672489,-21.9187953038495,-6.));
#10748=CARTESIAN_POINT('Origin',(83.,-23.,-6.));
#10749=CARTESIAN_POINT('Ctrl Pts',(81.7285261019851,-21.9187941775198,-6.));
#10750=CARTESIAN_POINT('Ctrl Pts',(82.0793422764381,-21.5073246555327,-6.03631814560907));
#10751=CARTESIAN_POINT('Ctrl Pts',(82.6492094739697,-21.281282050469,-6.07263629121814));
#10752=CARTESIAN_POINT('Ctrl Pts',(83.1865491620181,-21.3418040640572,-6.10895443682721));
#10753=CARTESIAN_POINT('Ctrl Pts',(83.7346336337695,-21.403536291519,-6.14599880949106));
#10754=CARTESIAN_POINT('Ctrl Pts',(84.2488767328762,-21.7634081614138,-6.18304318215492));
#10755=CARTESIAN_POINT('Ctrl Pts',(84.4942853325427,-22.257154116884,-6.22008755481877));
#10756=CARTESIAN_POINT('Ctrl Pts',(84.7396939322092,-22.7509000723541,-6.25713192748263));
#10757=CARTESIAN_POINT('Ctrl Pts',(84.7162680324355,-23.3785201133997,-6.29417630014648));
#10758=CARTESIAN_POINT('Ctrl Pts',(84.4345602306372,-23.8525938579917,-6.33122067281033));
#10759=CARTESIAN_POINT('Ctrl Pts',(84.1528524288388,-24.3266676025837,-6.36826504547418));
#10760=CARTESIAN_POINT('Ctrl Pts',(83.6128627250159,-24.6471950507222,-6.40530941813804));
#10761=CARTESIAN_POINT('Ctrl Pts',(83.0617850263329,-24.6676013026721,-6.44235379080189));
#10762=CARTESIAN_POINT('Ctrl Pts',(82.5107073276499,-24.6880075546221,-6.47939816346575));
#10763=CARTESIAN_POINT('Ctrl Pts',(81.948541634107,-24.4082926103835,-6.5164425361296));
#10764=CARTESIAN_POINT('Ctrl Pts',(81.6325039196586,-23.9564070095206,-6.55348690879346));
#10765=CARTESIAN_POINT('Ctrl Pts',(81.4391457526553,-23.6799344004507,-6.57615139365904));
#10766=CARTESIAN_POINT('Ctrl Pts',(81.337919098353,-23.3390142503256,-6.59881587852463));
#10767=CARTESIAN_POINT('Ctrl Pts',(81.3361555725406,-22.9990558295284,-6.62148036339021));
#10768=CARTESIAN_POINT('Origin',(83.,-23.,-4.45407471946233));
#10769=CARTESIAN_POINT('',(80.9445918241665,-22.9981768120733,-16.6459252805377));
#10770=CARTESIAN_POINT('',(80.9470732705607,-23.0015060107516,-16.7040747194623));
#10771=CARTESIAN_POINT('',(80.94525,-22.9999999999999,-4.45407471946233));
#10772=CARTESIAN_POINT('',(84.8174278887595,-22.0413794120407,-17.));
#10773=CARTESIAN_POINT('Ctrl Pts',(80.9470732705607,-23.0015060107516,-16.7040747194623));
#10774=CARTESIAN_POINT('Ctrl Pts',(80.9500635605842,-22.5475808384988,-16.7286277343139));
#10775=CARTESIAN_POINT('Ctrl Pts',(81.3216916635813,-21.4040173658448,-16.7902251218292));
#10776=CARTESIAN_POINT('Ctrl Pts',(83.2159924080748,-20.5820415540093,-16.8888668820084));
#10777=CARTESIAN_POINT('Ctrl Pts',(84.4986774253636,-21.4370673526013,-16.9629556273361));
#10778=CARTESIAN_POINT('Ctrl Pts',(84.8174278887595,-22.0413794120407,-17.));
#10779=CARTESIAN_POINT('',(85.0570979189415,-23.0754558306091,-17.));
#10780=CARTESIAN_POINT('Origin',(83.,-23.,-17.));
#10781=CARTESIAN_POINT('Ctrl Pts',(80.9445918241665,-22.9981768120733,-16.6459252805377));
#10782=CARTESIAN_POINT('Ctrl Pts',(80.9432972488844,-22.8578132508263,-16.6535432960884));
#10783=CARTESIAN_POINT('Ctrl Pts',(81.020425579335,-22.0363086702384,-16.6982056843029));
#10784=CARTESIAN_POINT('Ctrl Pts',(82.1263744182192,-20.7340408632062,-16.7799124451812));
#10785=CARTESIAN_POINT('Ctrl Pts',(84.4138509810425,-21.0348853436204,-16.890319336118));
#10786=CARTESIAN_POINT('Ctrl Pts',(85.0806816672165,-22.4089784863789,-16.9636818543909));
#10787=CARTESIAN_POINT('Ctrl Pts',(85.0571001899048,-23.0754560264203,-17.));
#10788=CARTESIAN_POINT('Origin',(83.,-23.,-4.45407471946233));
#10789=CARTESIAN_POINT('',(80.9485827974856,-23.0000495903536,-15.9459252805377));
#10790=CARTESIAN_POINT('',(80.9419860077008,-23.0004830909235,-16.0040747194623));
#10791=CARTESIAN_POINT('',(80.94525,-22.9999999999999,-4.45407471946233));
#10792=CARTESIAN_POINT('Ctrl Pts',(80.9419860077008,-23.0004830909235,-16.0040747194623));
#10793=CARTESIAN_POINT('Ctrl Pts',(80.9440550409229,-22.346392379771,-16.0396948316641));
#10794=CARTESIAN_POINT('Ctrl Pts',(81.6350687429363,-21.0082839131029,-16.1123593165297));
#10795=CARTESIAN_POINT('Ctrl Pts',(83.9141747133152,-20.7500128153374,-16.2220681740591));
#10796=CARTESIAN_POINT('Ctrl Pts',(85.3860298428717,-22.5475930446421,-16.3332012920507));
#10797=CARTESIAN_POINT('Ctrl Pts',(84.6743955395297,-24.7593786616575,-16.4443344100422));
#10798=CARTESIAN_POINT('Ctrl Pts',(82.4296922229958,-25.3606230541752,-16.5554675280338));
#10799=CARTESIAN_POINT('Ctrl Pts',(81.0884939258943,-24.1462800951831,-16.6420476311738));
#10800=CARTESIAN_POINT('Ctrl Pts',(80.9455519591099,-23.2324406548646,-16.69158336165));
#10801=CARTESIAN_POINT('Ctrl Pts',(80.9470732705607,-23.0015060107516,-16.7040747194623));
#10802=CARTESIAN_POINT('Ctrl Pts',(80.9485827974856,-23.0000495903536,-15.9459252805377));
#10803=CARTESIAN_POINT('Ctrl Pts',(80.9486568158977,-22.6540999364258,-15.9646103934386));
#10804=CARTESIAN_POINT('Ctrl Pts',(81.195745621415,-21.6221842533796,-16.0203398790033));
#10805=CARTESIAN_POINT('Ctrl Pts',(82.8298598709625,-20.5773510168392,-16.1131137372319));
#10806=CARTESIAN_POINT('Ctrl Pts',(84.9430514548956,-21.5430599298187,-16.2242468552234));
#10807=CARTESIAN_POINT('Ctrl Pts',(85.2779271980639,-23.842211340369,-16.335379973215));
#10808=CARTESIAN_POINT('Ctrl Pts',(83.5278718822138,-25.37055054633,-16.4465130912065));
#10809=CARTESIAN_POINT('Ctrl Pts',(81.4479221613014,-24.7732038337887,-16.5500281936475));
#10810=CARTESIAN_POINT('Ctrl Pts',(80.9495924223287,-23.5403637177663,-16.6164989234245));
#10811=CARTESIAN_POINT('Ctrl Pts',(80.9445918241665,-22.9981768120733,-16.6459252805377));
#10812=CARTESIAN_POINT('Origin',(83.,-23.,-4.45407471946233));
#10813=CARTESIAN_POINT('',(80.9444683918153,-23.0018063316281,-15.2459252805377));
#10814=CARTESIAN_POINT('',(80.9457761200516,-22.9981345158697,-15.3040747194623));
#10815=CARTESIAN_POINT('',(80.94525,-22.9999999999999,-4.45407471946233));
#10816=CARTESIAN_POINT('Ctrl Pts',(80.9457761200516,-22.9981345158697,-15.3040747194623));
#10817=CARTESIAN_POINT('Ctrl Pts',(80.9441910027471,-22.8202139788124,-15.3137175563504));
#10818=CARTESIAN_POINT('Ctrl Pts',(81.0468090685297,-21.9605854226314,-15.3604047659024));
#10819=CARTESIAN_POINT('Ctrl Pts',(82.2507940745424,-20.6898346105816,-15.4441363481181));
#10820=CARTESIAN_POINT('Ctrl Pts',(84.5344925201404,-21.1175797670015,-15.5552694661097));
#10821=CARTESIAN_POINT('Ctrl Pts',(85.4137606299914,-23.2681888577979,-15.6664025841013));
#10822=CARTESIAN_POINT('Ctrl Pts',(84.0838647611703,-25.1733432517703,-15.7775357020929));
#10823=CARTESIAN_POINT('Ctrl Pts',(81.7619637210983,-25.0893637699614,-15.8886688200844));
#10824=CARTESIAN_POINT('Ctrl Pts',(80.9542067795097,-23.7329548423873,-15.9641818258742));
#10825=CARTESIAN_POINT('Ctrl Pts',(80.9419032779722,-23.0266367294426,-16.0026504590002));
#10826=CARTESIAN_POINT('Ctrl Pts',(80.9419860077008,-23.0004830909235,-16.0040747194623));
#10827=CARTESIAN_POINT('Ctrl Pts',(80.9444683918153,-23.0018063316281,-15.2459252805377));
#10828=CARTESIAN_POINT('Ctrl Pts',(80.949498810733,-22.4537399021428,-15.2756774907888));
#10829=CARTESIAN_POINT('Ctrl Pts',(81.4568946252713,-21.2150551659787,-15.3424740737037));
#10830=CARTESIAN_POINT('Ctrl Pts',(83.5486977575985,-20.6341799887301,-15.4463150292825));
#10831=CARTESIAN_POINT('Ctrl Pts',(85.2852062676543,-22.1778048794721,-15.5574481472741));
#10832=CARTESIAN_POINT('Ctrl Pts',(84.9302047132626,-24.4739350041461,-15.6685812652656));
#10833=CARTESIAN_POINT('Ctrl Pts',(82.8086025236948,-25.4210620022677,-15.7797143832572));
#10834=CARTESIAN_POINT('Ctrl Pts',(81.1894351825912,-24.3656514787605,-15.8721623883479));
#10835=CARTESIAN_POINT('Ctrl Pts',(80.9485100698943,-23.3399661643164,-15.9275660207747));
#10836=CARTESIAN_POINT('Ctrl Pts',(80.9485827974856,-23.0000495903536,-15.9459252805377));
#10837=CARTESIAN_POINT('Origin',(83.,-23.,-4.45407471946233));
#10838=CARTESIAN_POINT('',(80.9427068937054,-22.9988171296078,-14.5459252805377));
#10839=CARTESIAN_POINT('',(80.9483912189187,-23.0006513925548,-14.6040747194623));
#10840=CARTESIAN_POINT('',(80.94525,-22.9999999999999,-4.45407471946233));
#10841=CARTESIAN_POINT('Ctrl Pts',(80.9483912189187,-23.0006513925548,-14.6040747194623));
#10842=CARTESIAN_POINT('Ctrl Pts',(80.9494812471314,-22.6173024205259,-14.6247846537006));
#10843=CARTESIAN_POINT('Ctrl Pts',(81.2366609896803,-21.5467311614289,-14.6825389606028));
#10844=CARTESIAN_POINT('Ctrl Pts',(82.9621345897233,-20.571679876643,-14.7773376401688));
#10845=CARTESIAN_POINT('Ctrl Pts',(85.0195746168704,-21.6511149812732,-14.8884707581604));
#10846=CARTESIAN_POINT('Ctrl Pts',(85.2286204270596,-23.9651027282846,-14.9996038761519));
#10847=CARTESIAN_POINT('Ctrl Pts',(83.397945180368,-25.3957905088984,-15.1107369941435));
#10848=CARTESIAN_POINT('Ctrl Pts',(81.3935017093533,-24.699876881042,-15.2122272752469));
#10849=CARTESIAN_POINT('Ctrl Pts',(80.9502804634345,-23.5037218257036,-15.2766731836866));
#10850=CARTESIAN_POINT('Ctrl Pts',(80.9457761200516,-22.9981345158697,-15.3040747194623));
#10851=CARTESIAN_POINT('Ctrl Pts',(80.9427068937054,-22.9988171296078,-14.5459252805377));
#10852=CARTESIAN_POINT('Ctrl Pts',(80.9422306998785,-22.9294336755561,-14.5497002154751));
#10853=CARTESIAN_POINT('Ctrl Pts',(80.976896368521,-22.1796546331155,-14.5905195230764));
#10854=CARTESIAN_POINT('Ctrl Pts',(81.896614425227,-20.83650429601,-14.6683832033416));
#10855=CARTESIAN_POINT('Ctrl Pts',(84.2191696850261,-20.8995717888251,-14.7795163213332));
#10856=CARTESIAN_POINT('Ctrl Pts',(85.4258928578083,-22.8850338533659,-14.8906494393247));
#10857=CARTESIAN_POINT('Ctrl Pts',(84.4123434153425,-24.9757174587147,-15.0017825573163));
#10858=CARTESIAN_POINT('Ctrl Pts',(82.1061616690569,-25.2581466855875,-15.1129156753078));
#10859=CARTESIAN_POINT('Ctrl Pts',(81.0164469782457,-23.9515225379254,-15.1942965830483));
#10860=CARTESIAN_POINT('Ctrl Pts',(80.9432354537767,-23.1361354918168,-15.2386331181249));
#10861=CARTESIAN_POINT('Ctrl Pts',(80.9444683918153,-23.0018063316281,-15.2459252805377));
#10862=CARTESIAN_POINT('Origin',(83.,-23.,-4.45407471946233));
#10863=CARTESIAN_POINT('',(80.9480449299229,-22.998944875009,-13.8459252805377));
#10864=CARTESIAN_POINT('',(80.9433899630638,-23.0015207493961,-13.9040747194623));
#10865=CARTESIAN_POINT('',(80.94525,-22.9999999999999,-4.45407471946233));
#10866=CARTESIAN_POINT('Ctrl Pts',(80.9433899630638,-23.0015207493961,-13.9040747194623));
#10867=CARTESIAN_POINT('Ctrl Pts',(80.9482330971096,-22.4169498138078,-13.9358517510509));
#10868=CARTESIAN_POINT('Ctrl Pts',(81.5151172915851,-21.142699823015,-14.0046731553033));
#10869=CARTESIAN_POINT('Ctrl Pts',(83.6768128836446,-20.6675985082928,-14.1105389322194));
#10870=CARTESIAN_POINT('Ctrl Pts',(85.326617632413,-22.3035642232594,-14.221672050211));
#10871=CARTESIAN_POINT('Ctrl Pts',(84.8470103486162,-24.5769353722521,-14.3328051682026));
#10872=CARTESIAN_POINT('Ctrl Pts',(82.6769464973495,-25.4070332015704,-14.4439382861941));
#10873=CARTESIAN_POINT('Ctrl Pts',(81.1518516642612,-24.2899654019874,-14.5343614699474));
#10874=CARTESIAN_POINT('Ctrl Pts',(80.9475314866512,-23.3030082280256,-14.5877402810368));
#10875=CARTESIAN_POINT('Ctrl Pts',(80.9483912189187,-23.0006513925548,-14.6040747194623));
#10876=CARTESIAN_POINT('Ctrl Pts',(80.9480449299229,-22.9989448750091,-13.8459252805377));
#10877=CARTESIAN_POINT('Ctrl Pts',(80.9467671190122,-22.7243288838564,-13.8607673128254));
#10878=CARTESIAN_POINT('Ctrl Pts',(81.1259274427508,-21.7658950801937,-13.9126537177769));
#10879=CARTESIAN_POINT('Ctrl Pts',(82.5805008816194,-20.6078892424568,-14.0015844953923));
#10880=CARTESIAN_POINT('Ctrl Pts',(84.7821633068503,-21.3501311159715,-14.1127176133838));
#10881=CARTESIAN_POINT('Ctrl Pts',(85.3527197283046,-23.6023979303683,-14.2238507313754));
#10882=CARTESIAN_POINT('Ctrl Pts',(83.769974452434,-25.3033264487149,-14.3349838493669));
#10883=CARTESIAN_POINT('Ctrl Pts',(81.5602178471133,-24.9099904475101,-14.442342032421));
#10884=CARTESIAN_POINT('Ctrl Pts',(80.9469037079901,-23.6103107161358,-14.5126558428113));
#10885=CARTESIAN_POINT('Ctrl Pts',(80.9427068937054,-22.9988171296078,-14.5459252805377));
#10886=CARTESIAN_POINT('Origin',(83.,-23.,-4.45407471946233));
#10887=CARTESIAN_POINT('',(80.9465558469908,-23.0017537142658,-13.1459252805377));
#10888=CARTESIAN_POINT('',(80.9436612253546,-22.9983838582986,-13.2040747194623));
#10889=CARTESIAN_POINT('',(80.94525,-22.9999999999999,-4.45407471946233));
#10890=CARTESIAN_POINT('Ctrl Pts',(80.9436612253546,-22.9983838582986,-13.2040747194623));
#10891=CARTESIAN_POINT('Ctrl Pts',(80.9427400817188,-22.8916548014817,-13.2098744757372));
#10892=CARTESIAN_POINT('Ctrl Pts',(80.9988246572765,-22.1041931228359,-13.252718604676));
#10893=CARTESIAN_POINT('Ctrl Pts',(82.0161587924632,-20.7795881291394,-13.3326071062786));
#10894=CARTESIAN_POINT('Ctrl Pts',(84.3318253496949,-20.9691347568542,-13.4437402242701));
#10895=CARTESIAN_POINT('Ctrl Pts',(85.4285529267558,-23.0174091891753,-13.5548733422617));
#10896=CARTESIAN_POINT('Ctrl Pts',(84.3025732783284,-25.0497500463396,-13.6660064602532));
#10897=CARTESIAN_POINT('Ctrl Pts',(81.9844272968094,-25.2060789837275,-13.7771395782448));
#10898=CARTESIAN_POINT('Ctrl Pts',(80.9928404632344,-23.8759493553275,-13.8564956646478));
#10899=CARTESIAN_POINT('Ctrl Pts',(80.9425871681638,-23.098418865631,-13.898807378387));
#10900=CARTESIAN_POINT('Ctrl Pts',(80.9433899630638,-23.0015207493961,-13.9040747194623));
#10901=CARTESIAN_POINT('Ctrl Pts',(80.9465558469908,-23.0017537142658,-13.1459252805377));
#10902=CARTESIAN_POINT('Ctrl Pts',(80.9504435912746,-22.523241982595,-13.1718344101756));
#10903=CARTESIAN_POINT('Ctrl Pts',(81.3555436948577,-21.3546297745119,-13.2347879124773));
#10904=CARTESIAN_POINT('Ctrl Pts',(83.301369139264,-20.5901556007548,-13.3347857874429));
#10905=CARTESIAN_POINT('Ctrl Pts',(85.1880466821996,-21.946138005623,-13.4459189054345));
#10906=CARTESIAN_POINT('Ctrl Pts',(85.0721377809063,-24.2666563873492,-13.557052023426));
#10907=CARTESIAN_POINT('Ctrl Pts',(83.0597268239821,-25.4278809882634,-13.6681851414176));
#10908=CARTESIAN_POINT('Ctrl Pts',(81.2687132343068,-24.5086941725721,-13.7644762271215));
#10909=CARTESIAN_POINT('Ctrl Pts',(80.9499564196855,-23.4097456056731,-13.8237229401615));
#10910=CARTESIAN_POINT('Ctrl Pts',(80.9480449299229,-22.9989448750091,-13.8459252805377));
#10911=CARTESIAN_POINT('Origin',(83.,-23.,-4.45407471946233));
#10912=CARTESIAN_POINT('',(80.9418454336727,-23.0000233771379,-12.4459252805377));
#10913=CARTESIAN_POINT('',(80.9484735339094,-22.9995028191082,-12.5040747194623));
#10914=CARTESIAN_POINT('',(80.94525,-22.9999999999999,-4.45407471946233));
#10915=CARTESIAN_POINT('Ctrl Pts',(80.9484735339094,-22.9995028191082,-12.5040747194623));
#10916=CARTESIAN_POINT('Ctrl Pts',(80.9477974848827,-22.6872594927532,-12.5209415730874));
#10917=CARTESIAN_POINT('Ctrl Pts',(81.1614618092461,-21.6901193881101,-12.5748527993764));
#10918=CARTESIAN_POINT('Ctrl Pts',(82.711487771974,-20.588582762733,-12.6658083983292));
#10919=CARTESIAN_POINT('Ctrl Pts',(84.869428030581,-21.4497060806457,-12.7769415163207));
#10920=CARTESIAN_POINT('Ctrl Pts',(85.3163941756299,-23.7297194125255,-12.8880746343123));
#10921=CARTESIAN_POINT('Ctrl Pts',(83.6433051987559,-25.3418648165858,-12.9992077523039));
#10922=CARTESIAN_POINT('Ctrl Pts',(81.4994791114416,-24.8383664692076,-13.1045411140205));
#10923=CARTESIAN_POINT('Ctrl Pts',(80.9486236372523,-23.5733577502603,-13.1728301030734));
#10924=CARTESIAN_POINT('Ctrl Pts',(80.9436612253546,-22.9983838582986,-13.2040747194623));
#10925=CARTESIAN_POINT('Ctrl Pts',(80.94184556232,-23.0000233762546,-12.4459252805377));
#10926=CARTESIAN_POINT('Ctrl Pts',(80.9419597191148,-22.3211541232341,-12.4829015075258));
#10927=CARTESIAN_POINT('Ctrl Pts',(81.6804453873982,-20.9619516944595,-12.5569221071777));
#10928=CARTESIAN_POINT('Ctrl Pts',(83.9956695846244,-20.7848667162158,-12.6679870794935));
#10929=CARTESIAN_POINT('Ctrl Pts',(85.4010383313655,-22.6350502527901,-12.7791201974851));
#10930=CARTESIAN_POINT('Ctrl Pts',(84.6088822932929,-24.819250162293,-12.8902533154767));
#10931=CARTESIAN_POINT('Ctrl Pts',(82.3442138554089,-25.3384007182767,-13.0013864334682));
#10932=CARTESIAN_POINT('Ctrl Pts',(81.0677939069456,-24.0952790226387,-13.0866104218219));
#10933=CARTESIAN_POINT('Ctrl Pts',(80.9448849696581,-23.2074088056333,-13.1347900375117));
#10934=CARTESIAN_POINT('Ctrl Pts',(80.9465558469908,-23.0017537142658,-13.1459252805377));
#10935=CARTESIAN_POINT('Origin',(83.,-23.,-4.45407471946233));
#10936=CARTESIAN_POINT('',(80.9464876953405,-22.9982315273104,-11.7459252805377));
#10937=CARTESIAN_POINT('',(80.9454840271886,-23.0018778870529,-11.8040747194623));
#10938=CARTESIAN_POINT('',(80.94525,-22.9999999999999,-4.45407471946233));
#10939=CARTESIAN_POINT('Ctrl Pts',(80.9454840271886,-23.0018778870529,-11.8040747194623));
#10940=CARTESIAN_POINT('Ctrl Pts',(80.9501626083473,-22.486653624791,-11.8320086704377));
#10941=CARTESIAN_POINT('Ctrl Pts',(81.407470405066,-21.2807660753287,-11.8969869940768));
#10942=CARTESIAN_POINT('Ctrl Pts',(83.4322511364777,-20.6101608102379,-11.9990096903798));
#10943=CARTESIAN_POINT('Ctrl Pts',(85.2422274635415,-22.0669467326842,-12.1101428083714));
#10944=CARTESIAN_POINT('Ctrl Pts',(85.0000289627594,-24.3776997299966,-12.221275926363));
#10945=CARTESIAN_POINT('Ctrl Pts',(82.9273252348868,-25.4275277086832,-12.3324090443545));
#10946=CARTESIAN_POINT('Ctrl Pts',(81.2256188601819,-24.4334541577041,-12.426675308721));
#10947=CARTESIAN_POINT('Ctrl Pts',(80.9492822794177,-23.3730339946484,-12.4838972004236));
#10948=CARTESIAN_POINT('Ctrl Pts',(80.9484735339094,-22.9995028191082,-12.5040747194623));
#10949=CARTESIAN_POINT('Ctrl Pts',(80.9464876953406,-22.9982315273104,-11.7459252805377));
#10950=CARTESIAN_POINT('Ctrl Pts',(80.9448193421433,-22.7951106380881,-11.7569242322122));
#10951=CARTESIAN_POINT('Ctrl Pts',(81.0658211635465,-21.9098241257738,-11.8049675565505));
#10952=CARTESIAN_POINT('Ctrl Pts',(82.3356362554336,-20.6640217891469,-11.8900552535526));
#10953=CARTESIAN_POINT('Ctrl Pts',(84.6021947432545,-21.1748574325926,-12.0011883715442));
#10954=CARTESIAN_POINT('Ctrl Pts',(85.4023615402782,-23.356135390641,-12.1123214895358));
#10955=CARTESIAN_POINT('Ctrl Pts',(84.0037924996106,-25.2114642218224,-12.2234546075273));
#10956=CARTESIAN_POINT('Ctrl Pts',(81.6865130544115,-25.0427739548083,-12.3345877255189));
#10957=CARTESIAN_POINT('Ctrl Pts',(80.9424129421303,-23.6826458175463,-12.4087446165223));
#10958=CARTESIAN_POINT('Ctrl Pts',(80.9418453519337,-23.0012745045541,-12.4458571348619));
#10959=CARTESIAN_POINT('Ctrl Pts',(80.94184556232,-23.0000233762546,-12.4459252805377));
#10960=CARTESIAN_POINT('Origin',(83.,-23.,-4.45407471946233));
#10961=CARTESIAN_POINT('',(80.948083343573,-23.001020415448,-11.0459252805377));
#10962=CARTESIAN_POINT('',(80.9420996930937,-22.9993455607543,-11.1040747194623));
#10963=CARTESIAN_POINT('',(80.94525,-22.9999999999999,-4.45407471946233));
#10964=CARTESIAN_POINT('Ctrl Pts',(80.9420996930937,-22.9993455607543,-11.1040747194623));
#10965=CARTESIAN_POINT('Ctrl Pts',(80.9419498972546,-22.9634098758055,-11.106031395124));
#10966=CARTESIAN_POINT('Ctrl Pts',(80.959087622844,-22.2472747969947,-11.1450324434495));
#10967=CARTESIAN_POINT('Ctrl Pts',(81.7920501260224,-20.8930995515055,-11.2210778644389));
#10968=CARTESIAN_POINT('Ctrl Pts',(84.1149085188063,-20.8424200147847,-11.3322109824305));
#10969=CARTESIAN_POINT('Ctrl Pts',(85.4173587528071,-22.7664426020535,-11.443344100422));
#10970=CARTESIAN_POINT('Ctrl Pts',(84.5073471099255,-24.9042261126527,-11.5544772184136));
#10971=CARTESIAN_POINT('Ctrl Pts',(82.2177520634359,-25.2991869353425,-11.6656103364051));
#10972=CARTESIAN_POINT('Ctrl Pts',(81.039647370209,-24.0194952561807,-11.7488095034214));
#10973=CARTESIAN_POINT('Ctrl Pts',(80.9439581475414,-23.1699139195325,-11.7949642977738));
#10974=CARTESIAN_POINT('Ctrl Pts',(80.9454840271886,-23.0018778870529,-11.8040747194623));
#10975=CARTESIAN_POINT('Ctrl Pts',(80.948083343573,-23.001020415448,-11.0459252805377));
#10976=CARTESIAN_POINT('Ctrl Pts',(80.9499185724722,-22.5927222976639,-11.0679913295624));
#10977=CARTESIAN_POINT('Ctrl Pts',(81.2657181572716,-21.4963595529218,-11.1271017512509));
#10978=CARTESIAN_POINT('Ctrl Pts',(83.0508160094325,-20.571916162926,-11.2232565456033));
#10979=CARTESIAN_POINT('Ctrl Pts',(85.0674751504547,-21.7257473213969,-11.3343896635948));
#10980=CARTESIAN_POINT('Ctrl Pts',(85.1918996587519,-24.0458246854221,-11.4455227815864));
#10981=CARTESIAN_POINT('Ctrl Pts',(83.3102113270295,-25.4087221340905,-11.556655899578));
#10982=CARTESIAN_POINT('Ctrl Pts',(81.3589374844954,-24.6503621653507,-11.656790065895));
#10983=CARTESIAN_POINT('Ctrl Pts',(80.9504383410627,-23.4792200094962,-11.7198798595483));
#10984=CARTESIAN_POINT('Ctrl Pts',(80.9464876953406,-22.9982315273104,-11.7459252805377));
#10985=CARTESIAN_POINT('Origin',(83.,-23.,-4.45407471946233));
#10986=CARTESIAN_POINT('',(80.9427634779915,-23.0012177328999,-10.3459252805377));
#10987=CARTESIAN_POINT('',(80.9474131382961,-22.998536475434,-10.4040747194623));
#10988=CARTESIAN_POINT('',(80.94525,-22.9999999999999,-4.45407471946233));
#10989=CARTESIAN_POINT('Ctrl Pts',(80.9474131382961,-22.998536475434,-10.4040747194623));
#10990=CARTESIAN_POINT('Ctrl Pts',(80.9458280534013,-22.7577490701563,-10.4170984924742));
#10991=CARTESIAN_POINT('Ctrl Pts',(81.0963188906304,-21.8339922531296,-10.46716663815));
#10992=CARTESIAN_POINT('Ctrl Pts',(82.4639279853743,-20.6312874397589,-10.5542791564896));
#10993=CARTESIAN_POINT('Ctrl Pts',(84.699278862516,-21.2648850916105,-10.6654122744811));
#10994=CARTESIAN_POINT('Ctrl Pts',(85.3793828417187,-23.4865282010775,-10.7765453924727));
#10995=CARTESIAN_POINT('Ctrl Pts',(83.8817819925845,-25.2628815513549,-10.8876785104643));
#10996=CARTESIAN_POINT('Ctrl Pts',(81.6177164603555,-24.973345741473,-10.9968549527941));
#10997=CARTESIAN_POINT('Ctrl Pts',(80.9447858771748,-23.6437550813218,-11.0689870224602));
#10998=CARTESIAN_POINT('Ctrl Pts',(80.9420996930937,-22.9993455607543,-11.1040747194623));
#10999=CARTESIAN_POINT('Ctrl Pts',(80.9427634779915,-23.0012177328999,-10.3459252805377));
#11000=CARTESIAN_POINT('Ctrl Pts',(80.9470399224638,-22.3921851286143,-10.3790584269126));
#11001=CARTESIAN_POINT('Ctrl Pts',(81.5560212459934,-21.0947968361722,-10.4492359459513));
#11002=CARTESIAN_POINT('Ctrl Pts',(83.7615159742851,-20.6938632287777,-10.5564578376539));
#11003=CARTESIAN_POINT('Ctrl Pts',(85.3504930611994,-22.3889715588227,-10.6675909556455));
#11004=CARTESIAN_POINT('Ctrl Pts',(84.7882063839989,-24.6433171680781,-10.778724073637));
#11005=CARTESIAN_POINT('Ctrl Pts',(82.5892828410451,-25.3936342247751,-10.8898571916286));
#11006=CARTESIAN_POINT('Ctrl Pts',(81.1282335614878,-24.2392080086894,-10.9789242605955));
#11007=CARTESIAN_POINT('Ctrl Pts',(80.9468375993813,-23.278171134301,-11.0309469568985));
#11008=CARTESIAN_POINT('Ctrl Pts',(80.948083343573,-23.001020415448,-11.0459252805377));
#11009=CARTESIAN_POINT('Origin',(83.,-23.,-4.45407471946233));
#11010=CARTESIAN_POINT('',(80.944392748711,-22.9982061753951,-9.64592528053768));
#11011=CARTESIAN_POINT('',(80.9473845690181,-23.0014769893773,-9.70407471946233));
#11012=CARTESIAN_POINT('',(80.94525,-22.9999999999999,-4.45407471946233));
#11013=CARTESIAN_POINT('Ctrl Pts',(80.9473845690181,-23.0014769893773,-9.70407471946233));
#11014=CARTESIAN_POINT('Ctrl Pts',(80.9503462238683,-22.5560933688278,-9.72816558982444));
#11015=CARTESIAN_POINT('Ctrl Pts',(81.3116443464902,-21.4214699850473,-9.78930083285041));
#11016=CARTESIAN_POINT('Ctrl Pts',(83.1830643685562,-20.5782940238596,-9.88748044854021));
#11017=CARTESIAN_POINT('Ctrl Pts',(85.1338458058857,-21.8403127686255,-9.99861356653179));
#11018=CARTESIAN_POINT('Ctrl Pts',(85.131647574316,-24.1637229123899,-10.1097466845233));
#11019=CARTESIAN_POINT('Ctrl Pts',(83.1784815819015,-25.4220480430476,-10.2208798025149));
#11020=CARTESIAN_POINT('Ctrl Pts',(81.3099987037936,-24.5759384329199,-10.3189891474946));
#11021=CARTESIAN_POINT('Ctrl Pts',(80.9503366144376,-23.4426364960753,-10.3800541198104));
#11022=CARTESIAN_POINT('Ctrl Pts',(80.9474131382961,-22.998536475434,-10.4040747194623));
#11023=CARTESIAN_POINT('Ctrl Pts',(80.944392748711,-22.9982061753951,-9.64592528053768));
#11024=CARTESIAN_POINT('Ctrl Pts',(80.9431863080667,-22.8664001375128,-9.65308115159894));
#11025=CARTESIAN_POINT('Ctrl Pts',(81.014785138996,-22.053568649942,-9.69728139532405));
#11026=CARTESIAN_POINT('Ctrl Pts',(82.0978802191083,-20.7451489433667,-9.77852601171301));
#11027=CARTESIAN_POINT('Ctrl Pts',(84.4050829423841,-21.0191124939321,-9.88965912970458));
#11028=CARTESIAN_POINT('Ctrl Pts',(85.4262984532635,-23.1060622570228,-10.0007922476961));
#11029=CARTESIAN_POINT('Ctrl Pts',(84.2268701215403,-25.0959396679168,-10.1119253656877));
#11030=CARTESIAN_POINT('Ctrl Pts',(81.9045619654454,-25.1675305993517,-10.2230584836792));
#11031=CARTESIAN_POINT('Ctrl Pts',(80.9783022134605,-23.8254196017566,-10.3010584552959));
#11032=CARTESIAN_POINT('Ctrl Pts',(80.9422586620029,-23.0731114282876,-10.3420140542487));
#11033=CARTESIAN_POINT('Ctrl Pts',(80.9427634779915,-23.0012177328999,-10.3459252805377));
#11034=CARTESIAN_POINT('Origin',(83.,-23.,-4.45407471946233));
#11035=CARTESIAN_POINT('',(80.9485808123477,-22.9999091152425,-8.94592528053768));
#11036=CARTESIAN_POINT('',(80.9420825813087,-23.0006320364948,-9.00407471946233));
#11037=CARTESIAN_POINT('',(80.94525,-22.9999999999999,-4.45407471946233));
#11038=CARTESIAN_POINT('Ctrl Pts',(80.9420825813087,-23.0006320364948,-9.00407471946233));
#11039=CARTESIAN_POINT('Ctrl Pts',(80.9446924463348,-22.3549462619531,-9.03923268717465));
#11040=CARTESIAN_POINT('Ctrl Pts',(81.6199953858007,-21.024225773533,-9.11143502755082));
#11041=CARTESIAN_POINT('Ctrl Pts',(83.886062338264,-20.7387910466673,-9.22068174059087));
#11042=CARTESIAN_POINT('Ctrl Pts',(85.3802992120524,-22.517975043166,-9.33181485858242));
#11043=CARTESIAN_POINT('Ctrl Pts',(84.695992559306,-24.7383272524714,-9.44294797657398));
#11044=CARTESIAN_POINT('Ctrl Pts',(82.4594467626664,-25.3676939404236,-9.55408109456554));
#11045=CARTESIAN_POINT('Ctrl Pts',(81.0952172934861,-24.1633756968917,-9.64112334219499));
#11046=CARTESIAN_POINT('Ctrl Pts',(80.9457921067143,-23.2409568283049,-9.69112121716059));
#11047=CARTESIAN_POINT('Ctrl Pts',(80.9473845690181,-23.0014769893773,-9.70407471946233));
#11048=CARTESIAN_POINT('Ctrl Pts',(80.9485808123477,-22.9999091152425,-8.94592528053768));
#11049=CARTESIAN_POINT('Ctrl Pts',(80.9484476854599,-22.6625169408995,-8.96414824894915));
#11050=CARTESIAN_POINT('Ctrl Pts',(81.1868156284612,-21.6394377060121,-9.01941559002448));
#11051=CARTESIAN_POINT('Ctrl Pts',(82.7997191561016,-20.5796568486397,-9.11172730376366));
#11052=CARTESIAN_POINT('Ctrl Pts',(84.9247819526336,-21.5189909448313,-9.22286042175521));
#11053=CARTESIAN_POINT('Ctrl Pts',(85.2882085474095,-23.8138028202287,-9.33399353974677));
#11054=CARTESIAN_POINT('Ctrl Pts',(83.5573766165987,-25.3637903236025,-9.44512665773833));
#11055=CARTESIAN_POINT('Ctrl Pts',(81.460707594627,-24.7898437540697,-9.54910390466863));
#11056=CARTESIAN_POINT('Ctrl Pts',(80.949431786282,-23.5487310438219,-9.61603677893508));
#11057=CARTESIAN_POINT('Ctrl Pts',(80.944392748711,-22.9982061753951,-9.64592528053768));
#11058=CARTESIAN_POINT('Origin',(83.,-23.,-4.45407471946233));
#11059=CARTESIAN_POINT('',(80.9447263139995,-23.0018413368225,-8.24592528053768));
#11060=CARTESIAN_POINT('',(80.9455228522428,-22.9981228933243,-8.30407471946232));
#11061=CARTESIAN_POINT('',(80.94525,-22.9999999999999,-4.45407471946233));
#11062=CARTESIAN_POINT('Ctrl Pts',(80.9455228522428,-22.9981228933243,-8.30407471946232));
#11063=CARTESIAN_POINT('Ctrl Pts',(80.9439883710969,-22.8287825981896,-8.31325541186101));
#11064=CARTESIAN_POINT('Ctrl Pts',(81.0405829332249,-21.9778760562739,-8.35948047692355));
#11065=CARTESIAN_POINT('Ctrl Pts',(82.2221040868968,-20.6993369771883,-8.44274991464995));
#11066=CARTESIAN_POINT('Ctrl Pts',(84.5109476719975,-21.0986295650073,-8.55388303264151));
#11067=CARTESIAN_POINT('Ctrl Pts',(85.4169124774121,-23.2381312128108,-8.66501615063307));
#11068=CARTESIAN_POINT('Ctrl Pts',(84.1108238547277,-25.1596858015617,-8.77614926862463));
#11069=CARTESIAN_POINT('Ctrl Pts',(81.7880655186073,-25.1046109404864,-8.88728238661618));
#11070=CARTESIAN_POINT('Ctrl Pts',(80.9584342768961,-23.7501147475331,-8.96325753689542));
#11071=CARTESIAN_POINT('Ctrl Pts',(80.9419425486894,-23.0352763837504,-9.0021883145108));
#11072=CARTESIAN_POINT('Ctrl Pts',(80.9420825813087,-23.0006320364948,-9.00407471946233));
#11073=CARTESIAN_POINT('Ctrl Pts',(80.9447263139995,-23.0018413368225,-8.24592528053768));
#11074=CARTESIAN_POINT('Ctrl Pts',(80.9497075994821,-22.4621139243731,-8.27521534629936));
#11075=CARTESIAN_POINT('Ctrl Pts',(81.4440784881194,-21.2316953680273,-8.3415497847249));
#11076=CARTESIAN_POINT('Ctrl Pts',(83.5192142592352,-20.6275350489011,-8.44492859581431));
#11077=CARTESIAN_POINT('Ctrl Pts',(85.2747978773029,-22.1494307757635,-8.55606171380584));
#11078=CARTESIAN_POINT('Ctrl Pts',(84.9483969412313,-24.4498009326555,-8.66719483179743));
#11079=CARTESIAN_POINT('Ctrl Pts',(82.8387464372207,-25.4232562134105,-8.77832794978897));
#11080=CARTESIAN_POINT('Ctrl Pts',(81.1984096379769,-24.382902257458,-8.87123809936907));
#11081=CARTESIAN_POINT('Ctrl Pts',(80.9487183110755,-23.3483811293246,-8.9271038762853));
#11082=CARTESIAN_POINT('Ctrl Pts',(80.9485808123477,-22.9999091152425,-8.94592528053768));
#11083=CARTESIAN_POINT('Origin',(83.,-23.,-4.45407471946233));
#11084=CARTESIAN_POINT('',(80.9425252865322,-22.9989407173183,-7.54592528053768));
#11085=CARTESIAN_POINT('',(80.948463949354,-23.0005177854378,-7.60407471946232));
#11086=CARTESIAN_POINT('',(80.94525,-22.9999999999999,-4.45407471946233));
#11087=CARTESIAN_POINT('Ctrl Pts',(80.948463949354,-23.0005177854378,-7.60407471946232));
#11088=CARTESIAN_POINT('Ctrl Pts',(80.949309331527,-22.6256901029336,-7.62432250921123));
#11089=CARTESIAN_POINT('Ctrl Pts',(81.2270645439503,-21.5639294398427,-7.68161467162399));
#11090=CARTESIAN_POINT('Ctrl Pts',(82.9319188416964,-20.5723391423155,-7.77595120670059));
#11091=CARTESIAN_POINT('Ctrl Pts',(85.0026323255168,-21.6260872678191,-7.88708432469216));
#11092=CARTESIAN_POINT('Ctrl Pts',(85.2404578851386,-23.9372944445138,-7.99821744268371));
#11093=CARTESIAN_POINT('Ctrl Pts',(83.4277282032368,-25.3906528329675,-8.10935056067527));
#11094=CARTESIAN_POINT('Ctrl Pts',(81.4056137883196,-24.716681927527,-8.21130298626814));
#11095=CARTESIAN_POINT('Ctrl Pts',(80.950180049126,-23.512075832246,-8.27621103919716));
#11096=CARTESIAN_POINT('Ctrl Pts',(80.9455228522428,-22.9981228933243,-8.30407471946232));
#11097=CARTESIAN_POINT('Ctrl Pts',(80.9425252865322,-22.9989407173183,-7.54592528053768));
#11098=CARTESIAN_POINT('Ctrl Pts',(80.9421428889425,-22.9380656487517,-7.54923807098573));
#11099=CARTESIAN_POINT('Ctrl Pts',(80.9722034692092,-22.1968547417379,-7.58959523409763));
#11100=CARTESIAN_POINT('Ctrl Pts',(81.8697768417376,-20.8504028018083,-7.66699676987338));
#11101=CARTESIAN_POINT('Ctrl Pts',(84.192936911971,-20.8845626742973,-7.77812988786495));
#11102=CARTESIAN_POINT('Ctrl Pts',(85.4242743751978,-22.854854309961,-7.8892630058565));
#11103=CARTESIAN_POINT('Ctrl Pts',(84.4368204072615,-24.9579888637226,-8.00039612384806));
#11104=CARTESIAN_POINT('Ctrl Pts',(82.1343319022801,-25.2690950090472,-8.11152924183961));
#11105=CARTESIAN_POINT('Ctrl Pts',(81.0221614548658,-23.9687902906062,-8.1933722940695));
#11106=CARTESIAN_POINT('Ctrl Pts',(80.9434075591455,-23.1447297834958,-8.23817097363551));
#11107=CARTESIAN_POINT('Ctrl Pts',(80.9447263139995,-23.0018413368225,-8.24592528053768));
#11108=CARTESIAN_POINT('Origin',(83.,-23.,-4.45407471946233));
#11109=CARTESIAN_POINT('',(80.9479085610311,-22.9988355136393,-6.84592528053768));
#11110=CARTESIAN_POINT('',(80.9436249062149,-23.0016062085623,-6.90407471946232));
#11111=CARTESIAN_POINT('',(80.94525,-22.9999999999999,-4.45407471946233));
#11112=CARTESIAN_POINT('Ctrl Pts',(80.9436249062148,-23.0016062085623,-6.90407471946232));
#11113=CARTESIAN_POINT('Ctrl Pts',(80.9485746682535,-22.4253659245422,-6.93538960656144));
#11114=CARTESIAN_POINT('Ctrl Pts',(81.5015294086587,-21.1591279528445,-7.00374886632441));
#11115=CARTESIAN_POINT('Ctrl Pts',(83.6477355304943,-20.659358138271,-7.10915249875124));
#11116=CARTESIAN_POINT('Ctrl Pts',(85.3177707839745,-22.2746643391349,-7.2202856167428));
#11117=CARTESIAN_POINT('Ctrl Pts',(84.8664911752114,-24.5538289281854,-7.33141873473436));
#11118=CARTESIAN_POINT('Ctrl Pts',(82.7069252853353,-25.4108667989543,-7.44255185272592));
#11119=CARTESIAN_POINT('Ctrl Pts',(81.1601824003909,-24.3072526384942,-7.53343718096857));
#11120=CARTESIAN_POINT('Ctrl Pts',(80.9477626613646,-23.3114566249889,-7.58727813654737));
#11121=CARTESIAN_POINT('Ctrl Pts',(80.948463949354,-23.0005177854378,-7.60407471946232));
#11122=CARTESIAN_POINT('Ctrl Pts',(80.9479085610311,-22.9988355136393,-6.84592528053768));
#11123=CARTESIAN_POINT('Ctrl Pts',(80.9465285725618,-22.7328123585093,-6.86030516833594));
#11124=CARTESIAN_POINT('Ctrl Pts',(81.118188380378,-21.7831881263893,-6.91172942879806));
#11125=CARTESIAN_POINT('Ctrl Pts',(82.550772583103,-20.6133039463769,-7.00019806192403));
#11126=CARTESIAN_POINT('Ctrl Pts',(84.7614902208339,-21.3280765684321,-7.11133117991559));
#11127=CARTESIAN_POINT('Ctrl Pts',(85.3600357932379,-23.5730756808161,-7.22246429790715));
#11128=CARTESIAN_POINT('Ctrl Pts',(83.7985771412431,-25.2935651717014,-7.33359741589871));
#11129=CARTESIAN_POINT('Ctrl Pts',(81.5745655362259,-24.9261854356127,-7.44141774344221));
#11130=CARTESIAN_POINT('Ctrl Pts',(80.9464189453495,-23.6187844449696,-7.51219369832188));
#11131=CARTESIAN_POINT('Ctrl Pts',(80.9425252865322,-22.9989407173183,-7.54592528053768));
#11132=CARTESIAN_POINT('Origin',(83.,-23.,-4.45407471946233));
#11133=CARTESIAN_POINT('',(80.9473274916068,-23.0023188026375,-6.14592528053767));
#11134=CARTESIAN_POINT('',(80.9434278273328,-22.9985036630511,-6.20407471946232));
#11135=CARTESIAN_POINT('',(80.94525,-22.9999999999999,-4.45407471946233));
#11136=CARTESIAN_POINT('',(82.4698297828114,-24.9851743256717,-6.));
#11137=CARTESIAN_POINT('Ctrl Pts',(82.4698297828114,-24.9851743256717,-6.));
#11138=CARTESIAN_POINT('Ctrl Pts',(81.8097404375819,-24.8088876857537,-6.03704437266385));
#11139=CARTESIAN_POINT('Ctrl Pts',(81.0750710560616,-24.1127868016837,-6.08568613284308));
#11140=CARTESIAN_POINT('Ctrl Pts',(80.9457104966695,-23.2165873425108,-6.1343278930223));
#11141=CARTESIAN_POINT('Ctrl Pts',(80.9473274916068,-23.0023188026375,-6.14592528053767));
#11142=CARTESIAN_POINT('',(83.5313111338805,-24.9887317157019,-5.99999999999999));
#11143=CARTESIAN_POINT('Origin',(83.,-23.,-6.));
#11144=CARTESIAN_POINT('Ctrl Pts',(83.5313118283826,-24.9887338811667,-6.));
#11145=CARTESIAN_POINT('Ctrl Pts',(82.8867914735066,-25.1600294862445,-6.03631814560907));
#11146=CARTESIAN_POINT('Ctrl Pts',(81.5070305341199,-24.840734884675,-6.10434305209651));
#11147=CARTESIAN_POINT('Ctrl Pts',(80.94828062884,-23.581675994672,-6.17236795858395));
#11148=CARTESIAN_POINT('Ctrl Pts',(80.9434278273328,-22.9985036630511,-6.20407471946232));
#11149=CARTESIAN_POINT('Origin',(83.,-23.,-17.));
#11150=CARTESIAN_POINT('Ctrl Pts',(82.2300979593296,-24.4774325188554,-17.));
#11151=CARTESIAN_POINT('Ctrl Pts',(82.2818390981198,-24.5125050767042,-17.));
#11152=CARTESIAN_POINT('Ctrl Pts',(82.3355567268774,-24.5443225394793,-17.));
#11153=CARTESIAN_POINT('Ctrl Pts',(82.3909195452282,-24.5729489534796,-17.));
#11154=CARTESIAN_POINT('Ctrl Pts',(82.4260295600056,-24.5911032644146,-17.));
#11155=CARTESIAN_POINT('Ctrl Pts',(82.4618021381845,-24.607973536627,-17.));
#11156=CARTESIAN_POINT('Ctrl Pts',(82.4981603817539,-24.6235688924305,-17.));
#11157=CARTESIAN_POINT('Ctrl Pts',(82.522943255033,-24.6341991564002,-17.));
#11158=CARTESIAN_POINT('Ctrl Pts',(82.5479983580097,-24.6442369519448,-17.));
#11159=CARTESIAN_POINT('Ctrl Pts',(82.5733025786055,-24.6536835842467,-17.));
#11160=CARTESIAN_POINT('Ctrl Pts',(82.5867931904283,-24.6587199317973,-17.));
#11161=CARTESIAN_POINT('Ctrl Pts',(82.6003545666375,-24.6635880767879,-17.));
#11162=CARTESIAN_POINT('Ctrl Pts',(82.6139694944138,-24.6682836926456,-17.));
#11163=CARTESIAN_POINT('Ctrl Pts',(82.6763337730807,-24.6897923411434,-17.));
#11164=CARTESIAN_POINT('Ctrl Pts',(82.7398893644175,-24.7077113174207,-17.));
#11165=CARTESIAN_POINT('Ctrl Pts',(82.8042863740348,-24.7220871703776,-17.));
#11166=CARTESIAN_POINT('Ctrl Pts',(82.8507390234662,-24.7324571621155,-17.));
#11167=CARTESIAN_POINT('Ctrl Pts',(82.8976303986295,-24.7409826885964,-17.));
#11168=CARTESIAN_POINT('Ctrl Pts',(82.9448382797826,-24.7476671912803,-17.));
#11169=CARTESIAN_POINT('Ctrl Pts',(82.9577357961264,-24.7494934431795,-17.));
#11170=CARTESIAN_POINT('Ctrl Pts',(82.9706569702704,-24.7511822070801,-17.));
#11171=CARTESIAN_POINT('Ctrl Pts',(82.983599376443,-24.7527333925106,-17.));
#11172=CARTESIAN_POINT('Ctrl Pts',(82.9969328091843,-24.7543314436251,-17.));
#11173=CARTESIAN_POINT('Ctrl Pts',(83.0102808606987,-24.7557824881839,-17.));
#11174=CARTESIAN_POINT('Ctrl Pts',(83.0236352576791,-24.7570864480777,-17.));
#11175=CARTESIAN_POINT('Ctrl Pts',(83.0911664152792,-24.763680375248,-17.));
#11176=CARTESIAN_POINT('Ctrl Pts',(83.1589012578161,-24.7665219197639,-17.));
#11177=CARTESIAN_POINT('Ctrl Pts',(83.2264851078505,-24.7656590371379,-17.));
#11178=CARTESIAN_POINT('Ctrl Pts',(83.2950476435056,-24.7647836590591,-17.));
#11179=CARTESIAN_POINT('Ctrl Pts',(83.3634557918544,-24.760096122702,-17.));
#11180=CARTESIAN_POINT('Ctrl Pts',(83.4313607347552,-24.7515982025416,-17.));
#11181=CARTESIAN_POINT('Ctrl Pts',(83.4734287914636,-24.7463336227933,-17.));
#11182=CARTESIAN_POINT('Ctrl Pts',(83.5153040865525,-24.73960565681,-17.));
#11183=CARTESIAN_POINT('Ctrl Pts',(83.5569050591773,-24.7314047821333,-17.));
#11184=CARTESIAN_POINT('Ctrl Pts',(83.5909684950016,-24.7246897956648,-17.));
#11185=CARTESIAN_POINT('Ctrl Pts',(83.6248480498378,-24.7169871539346,-17.));
#11186=CARTESIAN_POINT('Ctrl Pts',(83.6584986050691,-24.7082876471674,-17.));
#11187=CARTESIAN_POINT('Ctrl Pts',(83.6722821884436,-24.7047242475141,-17.));
#11188=CARTESIAN_POINT('Ctrl Pts',(83.6860298150871,-24.7009927099034,-17.));
#11189=CARTESIAN_POINT('Ctrl Pts',(83.6997151251742,-24.6970992429687,-17.));
#11190=CARTESIAN_POINT('Ctrl Pts',(83.7675104829974,-24.6778114824186,-17.));
#11191=CARTESIAN_POINT('Ctrl Pts',(83.8338962305779,-24.6545245448285,-17.));
#11192=CARTESIAN_POINT('Ctrl Pts',(83.8985096339753,-24.6272571466379,-17.));
#11193=CARTESIAN_POINT('Ctrl Pts',(83.9056765518862,-24.6242326471657,-17.));
#11194=CARTESIAN_POINT('Ctrl Pts',(83.9128216721735,-24.6211591229274,-17.));
#11195=CARTESIAN_POINT('Ctrl Pts',(83.9199445039688,-24.6180365600954,-17.));
#11196=CARTESIAN_POINT('Ctrl Pts',(83.9816971879894,-24.5909649344499,-17.));
#11197=CARTESIAN_POINT('Ctrl Pts',(84.0417754148873,-24.5602117258275,-17.));
#11198=CARTESIAN_POINT('Ctrl Pts',(84.1000372506631,-24.5260871320529,-17.));
#11199=CARTESIAN_POINT('Ctrl Pts',(84.1627131029041,-24.4893772006076,-17.));
#11200=CARTESIAN_POINT('Ctrl Pts',(84.2232879180125,-24.4487656795587,-17.));
#11201=CARTESIAN_POINT('Ctrl Pts',(84.2815651125216,-24.4045776673306,-17.));
#11202=CARTESIAN_POINT('Ctrl Pts',(84.2920907285267,-24.3965967400973,-17.));
#11203=CARTESIAN_POINT('Ctrl Pts',(84.3025413203083,-24.3884989956002,-17.));
#11204=CARTESIAN_POINT('Ctrl Pts',(84.3129156246037,-24.3802861603243,-17.));
#11205=CARTESIAN_POINT('Ctrl Pts',(84.3220913046107,-24.3730222179629,-17.));
#11206=CARTESIAN_POINT('Ctrl Pts',(84.3312003064953,-24.3656737636397,-17.));
#11207=CARTESIAN_POINT('Ctrl Pts',(84.3402399813965,-24.3582440922858,-17.));
#11208=CARTESIAN_POINT('Ctrl Pts',(84.395143202012,-24.3131193627022,-17.));
#11209=CARTESIAN_POINT('Ctrl Pts',(84.447514283769,-24.2649838963252,-17.));
#11210=CARTESIAN_POINT('Ctrl Pts',(84.4972032115259,-24.2141876925674,-17.));
#11211=CARTESIAN_POINT('Ctrl Pts',(84.547939867273,-24.1623204130814,-17.));
#11212=CARTESIAN_POINT('Ctrl Pts',(84.5958808308285,-24.107678464869,-17.));
#11213=CARTESIAN_POINT('Ctrl Pts',(84.6408461878852,-24.050583168076,-17.));
#11214=CARTESIAN_POINT('Ctrl Pts',(84.6860842877404,-23.9931415528714,-17.));
#11215=CARTESIAN_POINT('Ctrl Pts',(84.7283113614493,-23.9332160077481,-17.));
#11216=CARTESIAN_POINT('Ctrl Pts',(84.7673122483243,-23.8710921936606,-17.));
#11217=CARTESIAN_POINT('Ctrl Pts',(84.7769393443201,-23.8557573648973,-17.));
#11218=CARTESIAN_POINT('Ctrl Pts',(84.7863696800929,-23.840288425334,-17.));
#11219=CARTESIAN_POINT('Ctrl Pts',(84.7955996348862,-23.8246893660786,-17.));
#11220=CARTESIAN_POINT('Ctrl Pts',(84.8028491435325,-23.8124373542888,-17.));
#11221=CARTESIAN_POINT('Ctrl Pts',(84.8099757745391,-23.8001035206571,-17.));
#11222=CARTESIAN_POINT('Ctrl Pts',(84.8169673085382,-23.7877088770335,-17.));
#11223=CARTESIAN_POINT('Ctrl Pts',(84.8539824412826,-23.7220881736068,-17.));
#11224=CARTESIAN_POINT('Ctrl Pts',(84.8872834934608,-23.6546505166455,-17.));
#11225=CARTESIAN_POINT('Ctrl Pts',(84.9166897351286,-23.5857422245182,-17.));
#11226=CARTESIAN_POINT('Ctrl Pts',(84.9461280445966,-23.51675878721,-17.));
#11227=CARTESIAN_POINT('Ctrl Pts',(84.9716638092362,-23.4463006762683,-17.));
#11228=CARTESIAN_POINT('Ctrl Pts',(84.9930799698159,-23.3746776330315,-17.));
#11229=CARTESIAN_POINT('Ctrl Pts',(85.0140089050527,-23.3046840397455,-17.));
#11230=CARTESIAN_POINT('Ctrl Pts',(85.0310041061321,-23.233577039206,-17.));
#11231=CARTESIAN_POINT('Ctrl Pts',(85.043819389628,-23.1616224987288,-17.));
#11232=CARTESIAN_POINT('Ctrl Pts',(85.0465681982955,-23.1461886408205,-17.));
#11233=CARTESIAN_POINT('Ctrl Pts',(85.0491245173261,-23.1307157299229,-17.));
#11234=CARTESIAN_POINT('Ctrl Pts',(85.0514856095148,-23.115206305485,-17.));
#11235=CARTESIAN_POINT('Ctrl Pts',(85.0534987950829,-23.1019821926799,-17.));
#11236=CARTESIAN_POINT('Ctrl Pts',(85.0553700460339,-23.0887315335367,-17.));
#11237=CARTESIAN_POINT('Ctrl Pts',(85.0571001899048,-23.0754560264203,-17.));
#11238=CARTESIAN_POINT('Ctrl Pts',(84.8174278887595,-22.0413794120407,-17.));
#11239=CARTESIAN_POINT('Ctrl Pts',(84.7765814196328,-21.9788996623134,-17.));
#11240=CARTESIAN_POINT('Ctrl Pts',(84.7321382587602,-21.9189706353617,-17.));
#11241=CARTESIAN_POINT('Ctrl Pts',(84.6844272556429,-21.8617421036743,-17.));
#11242=CARTESIAN_POINT('Ctrl Pts',(84.6379676814808,-21.8060146396012,-17.));
#11243=CARTESIAN_POINT('Ctrl Pts',(84.5884084476132,-21.7528476571992,-17.));
#11244=CARTESIAN_POINT('Ctrl Pts',(84.53602713658,-21.7024171202736,-17.));
#11245=CARTESIAN_POINT('Ctrl Pts',(84.5243354623359,-21.6911608649784,-17.));
#11246=CARTESIAN_POINT('Ctrl Pts',(84.5125015270917,-21.6800396402157,-17.));
#11247=CARTESIAN_POINT('Ctrl Pts',(84.5005334026731,-21.6690603431566,-17.));
#11248=CARTESIAN_POINT('Ctrl Pts',(84.4456122010496,-21.618676827212,-17.));
#11249=CARTESIAN_POINT('Ctrl Pts',(84.3879772657735,-21.5713777924382,-17.));
#11250=CARTESIAN_POINT('Ctrl Pts',(84.3279447447431,-21.5273357256383,-17.));
#11251=CARTESIAN_POINT('Ctrl Pts',(84.2858002354275,-21.4964169625633,-17.));
#11252=CARTESIAN_POINT('Ctrl Pts',(84.2424734095645,-21.4671042688097,-17.));
#11253=CARTESIAN_POINT('Ctrl Pts',(84.1980683256475,-21.4394717254802,-17.));
#11254=CARTESIAN_POINT('Ctrl Pts',(84.1811929239341,-21.4289704443675,-17.));
#11255=CARTESIAN_POINT('Ctrl Pts',(84.1641617661438,-21.4187119484129,-17.));
#11256=CARTESIAN_POINT('Ctrl Pts',(84.1469804883186,-21.4087007908574,-17.));
#11257=CARTESIAN_POINT('Ctrl Pts',(84.1305957095552,-21.3991537360118,-17.));
#11258=CARTESIAN_POINT('Ctrl Pts',(84.1140690908491,-21.3898288825432,-17.));
#11259=CARTESIAN_POINT('Ctrl Pts',(84.0974351122763,-21.3807460873294,-17.));
#11260=CARTESIAN_POINT('Ctrl Pts',(84.033718117405,-21.3459541454306,-17.));
#11261=CARTESIAN_POINT('Ctrl Pts',(83.9683621660843,-21.314669355336,-17.));
#11262=CARTESIAN_POINT('Ctrl Pts',(83.9016589606957,-21.287053352088,-17.));
#11263=CARTESIAN_POINT('Ctrl Pts',(83.8363880887512,-21.2600303537011,-17.));
#11264=CARTESIAN_POINT('Ctrl Pts',(83.7698262768392,-21.2365201185219,-17.));
#11265=CARTESIAN_POINT('Ctrl Pts',(83.702238233304,-21.2167223499385,-17.));
#11266=CARTESIAN_POINT('Ctrl Pts',(83.6361325166137,-21.1973587818779,-17.));
#11267=CARTESIAN_POINT('Ctrl Pts',(83.5690443270263,-21.1815465129351,-17.));
#11268=CARTESIAN_POINT('Ctrl Pts',(83.5012252689848,-21.1695209782649,-17.));
#11269=CARTESIAN_POINT('Ctrl Pts',(83.4791651243258,-21.1656093191813,-17.));
#11270=CARTESIAN_POINT('Ctrl Pts',(83.457027727715,-21.1620987189897,-17.));
#11271=CARTESIAN_POINT('Ctrl Pts',(83.4348220326898,-21.1589984540086,-17.));
#11272=CARTESIAN_POINT('Ctrl Pts',(83.4223375091993,-21.1572554177768,-17.));
#11273=CARTESIAN_POINT('Ctrl Pts',(83.4098301119865,-21.1556420422429,-17.));
#11274=CARTESIAN_POINT('Ctrl Pts',(83.3973191364083,-21.1541618553483,-17.));
#11275=CARTESIAN_POINT('Ctrl Pts',(83.3294884653499,-21.1461367361461,-17.));
#11276=CARTESIAN_POINT('Ctrl Pts',(83.2614342665035,-21.1420048354048,-17.));
#11277=CARTESIAN_POINT('Ctrl Pts',(83.1934022649708,-21.1419441932168,-17.));
#11278=CARTESIAN_POINT('Ctrl Pts',(83.1836053465211,-21.1419354604652,-17.));
#11279=CARTESIAN_POINT('Ctrl Pts',(83.173808894589,-21.1420112428234,-17.));
#11280=CARTESIAN_POINT('Ctrl Pts',(83.1640136523952,-21.142172161946,-17.));
#11281=CARTESIAN_POINT('Ctrl Pts',(83.0946494144972,-21.1433116980679,-17.));
#11282=CARTESIAN_POINT('Ctrl Pts',(83.0253443835876,-21.1487165123659,-17.));
#11283=CARTESIAN_POINT('Ctrl Pts',(82.9564235651142,-21.1582133774548,-17.));
#11284=CARTESIAN_POINT('Ctrl Pts',(82.8921283089566,-21.1670728684926,-17.));
#11285=CARTESIAN_POINT('Ctrl Pts',(82.828166910253,-21.17949449625,-17.));
#11286=CARTESIAN_POINT('Ctrl Pts',(82.7648237414818,-21.1953720660214,-17.));
#11287=CARTESIAN_POINT('Ctrl Pts',(82.7509590903951,-21.1988473731343,-17.));
#11288=CARTESIAN_POINT('Ctrl Pts',(82.7371241565956,-21.2024883622745,-17.));
#11289=CARTESIAN_POINT('Ctrl Pts',(82.7233220999365,-21.2062940979554,-17.));
#11290=CARTESIAN_POINT('Ctrl Pts',(82.7122616849786,-21.209343861979,-17.));
#11291=CARTESIAN_POINT('Ctrl Pts',(82.7012229288043,-21.2124993619089,-17.));
#11292=CARTESIAN_POINT('Ctrl Pts',(82.6902205125981,-21.2157559907085,-17.));
#11293=CARTESIAN_POINT('Ctrl Pts',(82.6246583197173,-21.2351618849685,-17.));
#11294=CARTESIAN_POINT('Ctrl Pts',(82.5602625039766,-21.2581877772728,-17.));
#11295=CARTESIAN_POINT('Ctrl Pts',(82.4973355231435,-21.2846516488133,-17.));
#11296=CARTESIAN_POINT('Ctrl Pts',(82.4346998948261,-21.3109929923786,-17.));
#11297=CARTESIAN_POINT('Ctrl Pts',(82.3735186391274,-21.3407412554097,-17.));
#11298=CARTESIAN_POINT('Ctrl Pts',(82.3141198251038,-21.3737584862197,-17.));
#11299=CARTESIAN_POINT('Ctrl Pts',(82.2559937181132,-21.406068274254,-17.));
#11300=CARTESIAN_POINT('Ctrl Pts',(82.1995738158673,-21.4415091484104,-17.));
#11301=CARTESIAN_POINT('Ctrl Pts',(82.1452074852454,-21.479981235296,-17.));
#11302=CARTESIAN_POINT('Ctrl Pts',(82.1337109572647,-21.4881167010943,-17.));
#11303=CARTESIAN_POINT('Ctrl Pts',(82.1223064242023,-21.4963877994906,-17.));
#11304=CARTESIAN_POINT('Ctrl Pts',(82.1109974490861,-21.5047937147772,-17.));
#11305=CARTESIAN_POINT('Ctrl Pts',(82.1003663825044,-21.5126957434026,-17.));
#11306=CARTESIAN_POINT('Ctrl Pts',(82.0898185292626,-21.5207180219682,-17.));
#11307=CARTESIAN_POINT('Ctrl Pts',(82.0793734282098,-21.5288466119773,-17.));
#11308=CARTESIAN_POINT('Ctrl Pts',(82.0278060377264,-21.5689774037198,-17.));
#11309=CARTESIAN_POINT('Ctrl Pts',(81.9786452211898,-21.6117656835976,-17.));
#11310=CARTESIAN_POINT('Ctrl Pts',(81.9321820573122,-21.6570794404074,-17.));
#11311=CARTESIAN_POINT('Ctrl Pts',(81.8866025322933,-21.7015314178417,-17.));
#11312=CARTESIAN_POINT('Ctrl Pts',(81.8436184450026,-21.7484143885941,-17.));
#11313=CARTESIAN_POINT('Ctrl Pts',(81.8035470978193,-21.7976294922613,-17.));
#11314=CARTESIAN_POINT('Ctrl Pts',(81.7647768670758,-21.8452465817621,-17.));
#11315=CARTESIAN_POINT('Ctrl Pts',(81.7287329529628,-21.8950473870754,-17.));
#11316=CARTESIAN_POINT('Ctrl Pts',(81.6957494077667,-21.9469577312498,-17.));
#11317=CARTESIAN_POINT('Ctrl Pts',(81.6902971226995,-21.9555386764662,-17.));
#11318=CARTESIAN_POINT('Ctrl Pts',(81.6849285755936,-21.9641772894425,-17.));
#11319=CARTESIAN_POINT('Ctrl Pts',(81.6796454131484,-21.9728732610623,-17.));
#11320=CARTESIAN_POINT('Ctrl Pts',(81.6739898323046,-21.9821822253468,-17.));
#11321=CARTESIAN_POINT('Ctrl Pts',(81.6684320988345,-21.991556920899,-17.));
#11322=CARTESIAN_POINT('Ctrl Pts',(81.6629726161762,-22.000995687242,-17.));
#11323=CARTESIAN_POINT('Origin',(83.,-23.,-4.45407471946233));
#11324=CARTESIAN_POINT('Ctrl Pts',(80.9434278273328,-22.9985036630511,-6.20407471946232));
#11325=CARTESIAN_POINT('Ctrl Pts',(80.9426108920862,-22.9003306733166,-6.20941233124781));
#11326=CARTESIAN_POINT('Ctrl Pts',(80.9936360510926,-22.1216407869118,-6.25179431569714));
#11327=CARTESIAN_POINT('Ctrl Pts',(81.9885905792076,-20.7918186937154,-6.33122067281033));
#11328=CARTESIAN_POINT('Ctrl Pts',(84.3064560817636,-20.952810958716,-6.44235379080188));
#11329=CARTESIAN_POINT('Ctrl Pts',(85.4285782577618,-22.9871398469054,-6.55348690879345));
#11330=CARTESIAN_POINT('Ctrl Pts',(84.3279817091015,-25.0334050191953,-6.664620026785));
#11331=CARTESIAN_POINT('Ctrl Pts',(82.0119581717988,-25.218534557138,-6.77575314477657));
#11332=CARTESIAN_POINT('Ctrl Pts',(80.9980258697689,-23.8931863027124,-6.855571375669));
#11333=CARTESIAN_POINT('Ctrl Pts',(80.9427192797612,-23.107037225403,-6.89834523389759));
#11334=CARTESIAN_POINT('Ctrl Pts',(80.9436249062148,-23.0016062085623,-6.90407471946232));
#11335=CARTESIAN_POINT('Ctrl Pts',(80.9473274916068,-23.0023188026375,-6.14592528053767));
#11336=CARTESIAN_POINT('Ctrl Pts',(80.9508755015445,-22.5321708193339,-6.17137226568616));
#11337=CARTESIAN_POINT('Ctrl Pts',(81.3433671183963,-21.3705995282974,-6.23386362349849));
#11338=CARTESIAN_POINT('Ctrl Pts',(83.2718171975381,-20.587166548819,-6.33339935397468));
#11339=CARTESIAN_POINT('Ctrl Pts',(85.1745320976991,-21.9187032679059,-6.44453247196624));
#11340=CARTESIAN_POINT('Ctrl Pts',(85.0878555654783,-24.2409162559102,-6.55566558995779));
#11341=CARTESIAN_POINT('Ctrl Pts',(83.0898774551597,-25.4268774336938,-6.66679870794935));
#11342=CARTESIAN_POINT('Ctrl Pts',(81.2789895846428,-24.5258398827689,-6.76355193814265));
#11343=CARTESIAN_POINT('Ctrl Pts',(80.950083593842,-23.4181209669006,-6.82326079567209));
#11344=CARTESIAN_POINT('Ctrl Pts',(80.9479085610311,-22.9988355136393,-6.84592528053768));
#11345=CARTESIAN_POINT('Ctrl Pts',(84.2690708798524,-21.9206413469515,-6.));
#11346=CARTESIAN_POINT('Ctrl Pts',(84.627967898288,-22.3426194852432,-6.03704437266385));
#11347=CARTESIAN_POINT('Ctrl Pts',(84.8852397370454,-23.5657433557833,-6.11113311799156));
#11348=CARTESIAN_POINT('Ctrl Pts',(83.5452626210686,-24.8933533980037,-6.22226623598312));
#11349=CARTESIAN_POINT('Ctrl Pts',(81.7059923092724,-24.4836988369728,-6.33339935397468));
#11350=CARTESIAN_POINT('Ctrl Pts',(81.0511940946918,-22.718246934168,-6.44453247196624));
#11351=CARTESIAN_POINT('Ctrl Pts',(82.1799449592213,-21.2095972472222,-6.55566558995779));
#11352=CARTESIAN_POINT('Ctrl Pts',(84.059280122749,-21.3401304573407,-6.66679870794935));
#11353=CARTESIAN_POINT('Ctrl Pts',(84.9691015342163,-22.9895729334198,-6.77793182594091));
#11354=CARTESIAN_POINT('Ctrl Pts',(84.0767331925359,-24.6486933991869,-6.88906494393248));
#11355=CARTESIAN_POINT('Ctrl Pts',(82.1988915022347,-24.7987972124064,-7.00019806192403));
#11356=CARTESIAN_POINT('Ctrl Pts',(81.0542582228978,-23.302604896914,-7.11133117991558));
#11357=CARTESIAN_POINT('Ctrl Pts',(81.6904432068723,-21.5294396795688,-7.22246429790715));
#11358=CARTESIAN_POINT('Ctrl Pts',(83.5251867106965,-21.1021976680177,-7.33359741589871));
#11359=CARTESIAN_POINT('Ctrl Pts',(84.8792583653007,-22.4118947750328,-7.44473053389027));
#11360=CARTESIAN_POINT('Ctrl Pts',(84.5133589477561,-24.2598510740269,-7.55586365188182));
#11361=CARTESIAN_POINT('Ctrl Pts',(82.7623737804448,-24.9547410084233,-7.66699676987339));
#11362=CARTESIAN_POINT('Ctrl Pts',(81.2288735200345,-23.8605755728289,-7.77812988786494));
#11363=CARTESIAN_POINT('Ctrl Pts',(81.3163779059484,-21.9787772308784,-7.8892630058565));
#11364=CARTESIAN_POINT('Ctrl Pts',(82.9447995085857,-21.0316422976506,-8.00039612384807));
#11365=CARTESIAN_POINT('Ctrl Pts',(84.6237427688579,-21.8860257394752,-8.11152924183962));
#11366=CARTESIAN_POINT('Ctrl Pts',(84.8165727395747,-23.7599623042025,-8.22266235983119));
#11367=CARTESIAN_POINT('Ctrl Pts',(83.3468038382248,-24.9383514392134,-8.33379547782273));
#11368=CARTESIAN_POINT('Ctrl Pts',(81.5596264146683,-24.3426850528549,-8.44492859581431));
#11369=CARTESIAN_POINT('Ctrl Pts',(81.0907355886569,-22.5181404542583,-8.55606171380585));
#11370=CARTESIAN_POINT('Ctrl Pts',(82.3692786999733,-21.134612679886,-8.66719483179742));
#11371=CARTESIAN_POINT('Ctrl Pts',(84.2250827699467,-21.458360800731,-8.77832794978898));
#11372=CARTESIAN_POINT('Ctrl Pts',(84.9596428701148,-23.1930777956164,-8.88946106778053));
#11373=CARTESIAN_POINT('Ctrl Pts',(83.9006606847433,-24.7510823922139,-9.0005941857721));
#11374=CARTESIAN_POINT('Ctrl Pts',(82.017358391045,-24.7064274616622,-9.11172730376365));
#11375=CARTESIAN_POINT('Ctrl Pts',(81.0334083742546,-23.0999829537985,-9.22286042175522));
#11376=CARTESIAN_POINT('Ctrl Pts',(81.8493604176406,-21.4020301113619,-9.33399353974677));
#11377=CARTESIAN_POINT('Ctrl Pts',(83.7184230955337,-21.1666022064717,-9.44512665773833));
#11378=CARTESIAN_POINT('Ctrl Pts',(84.9299566795373,-22.6091721240612,-9.5562597757299));
#11379=CARTESIAN_POINT('Ctrl Pts',(84.3751179480734,-24.4094430965408,-9.66739289372144));
#11380=CARTESIAN_POINT('Ctrl Pts',(82.5617171464179,-24.9197362719288,-9.77852601171301));
#11381=CARTESIAN_POINT('Ctrl Pts',(81.1494500630057,-23.6730112511631,-9.88965912970457));
#11382=CARTESIAN_POINT('Ctrl Pts',(81.4308791188664,-21.8103198438688,-10.0007922476961));
#11383=CARTESIAN_POINT('Ctrl Pts',(83.1484293651367,-21.0364705408201,-10.1119253656877));
#11384=CARTESIAN_POINT('Ctrl Pts',(84.7301312143109,-22.0597206825795,-10.2230584836792));
#11385=CARTESIAN_POINT('Ctrl Pts',(84.7283488788469,-23.9435514646753,-10.3341916016708));
#11386=CARTESIAN_POINT('Ctrl Pts',(83.144713622313,-24.9638068084766,-10.4453247196624));
#11387=CARTESIAN_POINT('Ctrl Pts',(81.4286307627658,-24.1867088664773,-10.5564578376539));
#11388=CARTESIAN_POINT('Ctrl Pts',(81.1507268776256,-22.3234882614722,-10.6675909556455));
#11389=CARTESIAN_POINT('Ctrl Pts',(82.5653505407635,-21.0794378268102,-10.7787240736371));
#11390=CARTESIAN_POINT('Ctrl Pts',(84.3777824966304,-21.5931614856421,-10.8898571916286));
#11391=CARTESIAN_POINT('Ctrl Pts',(84.9292136825907,-23.3944791254386,-11.0009903096202));
#11392=CARTESIAN_POINT('Ctrl Pts',(83.7149525731334,-24.8347539430867,-11.1121234276117));
#11393=CARTESIAN_POINT('Ctrl Pts',(81.8463387284853,-24.5957897368103,-11.2232565456033));
#11394=CARTESIAN_POINT('Ctrl Pts',(81.0336010871927,-22.8962959537331,-11.3343896635948));
#11395=CARTESIAN_POINT('Ctrl Pts',(82.0205891276083,-21.2917161955509,-11.4455227815864));
#11396=CARTESIAN_POINT('Ctrl Pts',(83.9039725476732,-21.2506250125958,-11.556655899578));
#11397=CARTESIAN_POINT('Ctrl Pts',(84.9600047120946,-22.8106306728416,-11.6677890175695));
#11398=CARTESIAN_POINT('Ctrl Pts',(84.2221634189736,-24.5439545948068,-11.7789221355611));
#11399=CARTESIAN_POINT('Ctrl Pts',(82.3657500609242,-24.8641905021442,-11.8900552535526));
#11400=CARTESIAN_POINT('Ctrl Pts',(81.0898272109517,-23.478245888096,-12.0011883715442));
#11401=CARTESIAN_POINT('Ctrl Pts',(81.5621696811842,-21.6545918136877,-12.1123214895357));
#11402=CARTESIAN_POINT('Ctrl Pts',(83.3504710516471,-21.0623082661426,-12.2234546075273));
#11403=CARTESIAN_POINT('Ctrl Pts',(84.8180075212363,-22.2434764602272,-12.3345877255189));
#11404=CARTESIAN_POINT('Ctrl Pts',(84.6216319513115,-24.1170447743883,-12.4457208435104));
#11405=CARTESIAN_POINT('Ctrl Pts',(82.9410749927345,-24.9682497445753,-12.556853961502));
#11406=CARTESIAN_POINT('Ctrl Pts',(81.3144485200729,-24.018035078972,-12.6679870794935));
#11407=CARTESIAN_POINT('Ctrl Pts',(81.2305051045002,-22.1360746396232,-12.7791201974851));
#11408=CARTESIAN_POINT('Ctrl Pts',(82.7660730639293,-21.0448126938621,-12.8902533154767));
#11409=CARTESIAN_POINT('Ctrl Pts',(84.5157401625249,-21.7430151261009,-13.0013864334682));
#11410=CARTESIAN_POINT('Ctrl Pts',(84.8781422054261,-23.5916595893747,-13.1125195514598));
#11411=CARTESIAN_POINT('Ctrl Pts',(83.5215945789647,-24.8987939089582,-13.2236526694514));
#11412=CARTESIAN_POINT('Ctrl Pts',(81.687663064072,-24.4680773072633,-13.3347857874429));
#11413=CARTESIAN_POINT('Ctrl Pts',(81.0548339660191,-22.6937185710011,-13.4459189054345));
#11414=CARTESIAN_POINT('Ctrl Pts',(82.2022973832551,-21.1996806536787,-13.557052023426));
#11415=CARTESIAN_POINT('Ctrl Pts',(84.0798496326035,-21.3533658619876,-13.6681851414176));
#11416=CARTESIAN_POINT('Ctrl Pts',(84.9690809957294,-23.0141154442955,-13.7793182594091));
#11417=CARTESIAN_POINT('Ctrl Pts',(84.0561319292834,-24.6619460164019,-13.8904513774007));
#11418=CARTESIAN_POINT('Ctrl Pts',(82.1765693522251,-24.788698180747,-14.0015844953923));
#11419=CARTESIAN_POINT('Ctrl Pts',(81.0506429138938,-23.2783633675832,-14.1127176133838));
#11420=CARTESIAN_POINT('Ctrl Pts',(81.7088448067759,-21.5132594441617,-14.2238507313754));
#11421=CARTESIAN_POINT('Ctrl Pts',(83.5487627517468,-21.1088789949219,-14.3349838493669));
#11422=CARTESIAN_POINT('Ctrl Pts',(84.8864314274729,-22.4353269234458,-14.4461169673585));
#11423=CARTESIAN_POINT('Ctrl Pts',(84.4975638110693,-24.278585876711,-14.55725008535));
#11424=CARTESIAN_POINT('Ctrl Pts',(82.7380668522128,-24.9516327114326,-14.6683832033416));
#11425=CARTESIAN_POINT('Ctrl Pts',(81.2183014178553,-23.838468472195,-14.7795163213332));
#11426=CARTESIAN_POINT('Ctrl Pts',(81.3292166567263,-21.9579048872837,-14.8906494393247));
#11427=CARTESIAN_POINT('Ctrl Pts',(82.969298565022,-21.0311077622519,-15.0017825573163));
#11428=CARTESIAN_POINT('Ctrl Pts',(84.6374796504228,-21.9063183155134,-15.1129156753078));
#11429=CARTESIAN_POINT('Ctrl Pts',(84.8069748784432,-23.7825093784266,-15.2240487932994));
#11430=CARTESIAN_POINT('Ctrl Pts',(83.3226556371789,-24.9425170886116,-15.3351819112909));
#11431=CARTESIAN_POINT('Ctrl Pts',(81.5430291349163,-24.3246566433919,-15.4463150292825));
#11432=CARTESIAN_POINT('Ctrl Pts',(81.0968799579766,-22.4944184181754,-15.5574481472741));
#11433=CARTESIAN_POINT('Ctrl Pts',(82.3925406634323,-21.1269081208074,-15.6685812652656));
#11434=CARTESIAN_POINT('Ctrl Pts',(84.244173032512,-21.4737257047449,-15.7797143832572));
#11435=CARTESIAN_POINT('Ctrl Pts',(84.9570873388809,-23.2174486614387,-15.8908475012488));
#11436=CARTESIAN_POINT('Ctrl Pts',(83.8788021375398,-24.7621559106701,-16.0019806192403));
#11437=CARTESIAN_POINT('Ctrl Pts',(81.9961949431072,-24.6940649912425,-16.1131137372319));
#11438=CARTESIAN_POINT('Ctrl Pts',(81.0323249760943,-23.0755065351483,-16.2242468552234));
#11439=CARTESIAN_POINT('Ctrl Pts',(81.8693180677509,-21.3878267275145,-16.335379973215));
#11440=CARTESIAN_POINT('Ctrl Pts',(83.7412167282557,-21.1757008640235,-16.4465130912065));
#11441=CARTESIAN_POINT('Ctrl Pts',(84.9346030992696,-22.6331865250633,-16.5576462091981));
#11442=CARTESIAN_POINT('Ctrl Pts',(84.3576069929949,-24.4265116682426,-16.6687793271897));
#11443=CARTESIAN_POINT('Ctrl Pts',(82.5375920396697,-24.9140031674198,-16.7799124451812));
#11444=CARTESIAN_POINT('Ctrl Pts',(81.1417560182126,-23.6501903157134,-16.8910455631728));
#11445=CARTESIAN_POINT('Ctrl Pts',(81.4447231066816,-21.7903669148141,-17.0021786811644));
#11446=CARTESIAN_POINT('Ctrl Pts',(83.1751275589987,-21.0395090541329,-17.1133117991559));
#11447=CARTESIAN_POINT('Ctrl Pts',(84.2151340020225,-21.7327675918889,-17.1874005444836));
#11448=CARTESIAN_POINT('Ctrl Pts',(84.4735782273626,-22.2227463683951,-17.2244449171475));
#11449=CARTESIAN_POINT('Ctrl Pts',(84.3677806246588,-21.8366876301902,-5.92518502761751));
#11450=CARTESIAN_POINT('Ctrl Pts',(84.7545930524416,-22.2914876975058,-5.96222940028136));
#11451=CARTESIAN_POINT('Ctrl Pts',(85.0318757810182,-23.6097475033545,-6.03631814560907));
#11452=CARTESIAN_POINT('Ctrl Pts',(83.5876737543099,-25.0406205315519,-6.14745126360063));
#11453=CARTESIAN_POINT('Ctrl Pts',(81.6053429515753,-24.5991025830459,-6.25858438159219));
#11454=CARTESIAN_POINT('Ctrl Pts',(80.8996138034376,-22.6963318672728,-6.36971749958374));
#11455=CARTESIAN_POINT('Ctrl Pts',(82.1161601658834,-21.0703377293866,-6.48085061757531));
#11456=CARTESIAN_POINT('Ctrl Pts',(84.1416721090871,-21.2110239577992,-6.59198373556686));
#11457=CARTESIAN_POINT('Ctrl Pts',(85.1222604420648,-22.9887619045816,-6.70311685355843));
#11458=CARTESIAN_POINT('Ctrl Pts',(84.1604826980578,-24.7769306058564,-6.81424997154999));
#11459=CARTESIAN_POINT('Ctrl Pts',(82.1365803920894,-24.9387096606502,-6.92538308954154));
#11460=CARTESIAN_POINT('Ctrl Pts',(80.9029162629441,-23.3261418424273,-7.0365162075331));
#11461=CARTESIAN_POINT('Ctrl Pts',(81.5885844226929,-21.4150578619282,-7.14764932552466));
#11462=CARTESIAN_POINT('Ctrl Pts',(83.5660363172957,-20.9545844914355,-7.25878244351622));
#11463=CARTESIAN_POINT('Ctrl Pts',(85.0254291715253,-22.3661512964002,-7.36991556150778));
#11464=CARTESIAN_POINT('Ctrl Pts',(84.6310696902412,-24.3578436920797,-7.48104867949934));
#11465=CARTESIAN_POINT('Ctrl Pts',(82.7438909487416,-25.1067829386003,-7.5921817974909));
#11466=CARTESIAN_POINT('Ctrl Pts',(81.0911133321419,-23.9275120982265,-7.70331491548245));
#11467=CARTESIAN_POINT('Ctrl Pts',(81.1854239065361,-21.8993453878419,-7.81444803347402));
#11468=CARTESIAN_POINT('Ctrl Pts',(82.940505952956,-20.8785412458722,-7.92558115146558));
#11469=CARTESIAN_POINT('Ctrl Pts',(84.7500392877441,-21.7993795822564,-8.03671426945713));
#11470=CARTESIAN_POINT('Ctrl Pts',(84.957867788096,-23.8190730176396,-8.14784738744869));
#11471=CARTESIAN_POINT('Ctrl Pts',(83.3737786265622,-25.0891185704648,-8.25898050544025));
#11472=CARTESIAN_POINT('Ctrl Pts',(81.4475925548648,-24.4471205899292,-8.37011362343181));
#11473=CARTESIAN_POINT('Ctrl Pts',(80.942230878791,-22.4806608827483,-8.48124674142337));
#11474=CARTESIAN_POINT('Ctrl Pts',(82.3202204956144,-20.9895207789868,-8.59237985941492));
#11475=CARTESIAN_POINT('Ctrl Pts',(84.3203710706302,-21.3384503888231,-8.7035129774065));
#11476=CARTESIAN_POINT('Ctrl Pts',(85.1120660725473,-23.2080956013479,-8.81464609539804));
#11477=CARTESIAN_POINT('Ctrl Pts',(83.970715074738,-24.8872835286632,-8.9257792133896));
#11478=CARTESIAN_POINT('Ctrl Pts',(81.9409274335658,-24.839155287937,-9.03691233138117));
#11479=CARTESIAN_POINT('Ctrl Pts',(80.8804446898791,-23.1077597391704,-9.14804544937272));
#11480=CARTESIAN_POINT('Ctrl Pts',(81.7598623909015,-21.2777382357701,-9.25917856736428));
#11481=CARTESIAN_POINT('Ctrl Pts',(83.7743028431105,-21.0239984865369,-9.37031168535585));
#11482=CARTESIAN_POINT('Ctrl Pts',(85.0800708570423,-22.5787730970961,-9.4814448033474));
#11483=CARTESIAN_POINT('Ctrl Pts',(84.4820761518177,-24.5190711485177,-9.59257792133897));
#11484=CARTESIAN_POINT('Ctrl Pts',(82.5276270185007,-25.0690554947604,-9.70371103933051));
#11485=CARTESIAN_POINT('Ctrl Pts',(81.0055122302712,-23.7253588149665,-9.81484415732208));
#11486=CARTESIAN_POINT('Ctrl Pts',(81.3088311511714,-21.7177851978712,-9.92597727531363));
#11487=CARTESIAN_POINT('Ctrl Pts',(83.1599743662765,-20.8837450351666,-10.0371103933052));
#11488=CARTESIAN_POINT('Ctrl Pts',(84.8647027448359,-21.9865847112615,-10.1482435112968));
#11489=CARTESIAN_POINT('Ctrl Pts',(84.8627817773365,-24.0169419472468,-10.2593766292883));
#11490=CARTESIAN_POINT('Ctrl Pts',(83.1559696088426,-25.1165538866669,-10.3705097472799));
#11491=CARTESIAN_POINT('Ctrl Pts',(81.3064079154319,-24.2790124022603,-10.4816428652714));
#11492=CARTESIAN_POINT('Ctrl Pts',(81.0068883569529,-22.2708684258674,-10.592775983263));
#11493=CARTESIAN_POINT('Ctrl Pts',(82.5315430223004,-20.9300543644598,-10.7039091012546));
#11494=CARTESIAN_POINT('Ctrl Pts',(84.4849479519257,-21.4837360209649,-10.8150422192461));
#11495=CARTESIAN_POINT('Ctrl Pts',(85.0792700689667,-23.4251621506516,-10.9261753372377));
#11496=CARTESIAN_POINT('Ctrl Pts',(83.7705623796171,-24.9774631458428,-11.0373084552292));
#11497=CARTESIAN_POINT('Ctrl Pts',(81.7566056714021,-24.7199120377677,-11.1484415732208));
#11498=CARTESIAN_POINT('Ctrl Pts',(80.880652392244,-22.8882297376495,-11.2595746912124));
#11499=CARTESIAN_POINT('Ctrl Pts',(81.944409460413,-21.1588439808691,-11.3707078092039));
#11500=CARTESIAN_POINT('Ctrl Pts',(83.974284538051,-21.1145566799921,-11.4818409271955));
#11501=CARTESIAN_POINT('Ctrl Pts',(85.1124560589988,-22.7959013159122,-11.592974045187));
#11502=CARTESIAN_POINT('Ctrl Pts',(84.3172246492909,-24.6640451007554,-11.7041071631786));
#11503=CARTESIAN_POINT('Ctrl Pts',(82.3164173950948,-25.0091893132103,-11.8152402811701));
#11504=CARTESIAN_POINT('Ctrl Pts',(80.9412518464573,-23.5154443852944,-11.9263733991617));
#11505=CARTESIAN_POINT('Ctrl Pts',(81.4503336394796,-21.5499444682637,-12.0375065171532));
#11506=CARTESIAN_POINT('Ctrl Pts',(83.3777310799239,-20.9115924475077,-12.1486396351448));
#11507=CARTESIAN_POINT('Ctrl Pts',(84.9594141686714,-22.1846332177129,-12.2597727531364));
#11508=CARTESIAN_POINT('Ctrl Pts',(84.7477642884607,-24.2039297595911,-12.370905871128));
#11509=CARTESIAN_POINT('Ctrl Pts',(82.9364917401187,-25.1213423992779,-12.4820389891195));
#11510=CARTESIAN_POINT('Ctrl Pts',(81.1833444508808,-24.0972189799224,-12.5931721071111));
#11511=CARTESIAN_POINT('Ctrl Pts',(81.0928718230625,-22.0688775640237,-12.7043052251026));
#11512=CARTESIAN_POINT('Ctrl Pts',(82.747877966611,-20.8927360501525,-12.8154383430942));
#11513=CARTESIAN_POINT('Ctrl Pts',(84.6336361185435,-21.6452454442825,-12.9265714610857));
#11514=CARTESIAN_POINT('Ctrl Pts',(85.0242261954942,-23.637679530425,-13.0377045790773));
#11515=CARTESIAN_POINT('Ctrl Pts',(83.5621647855617,-25.0464842115007,-13.1488376970689));
#11516=CARTESIAN_POINT('Ctrl Pts',(81.585588037293,-24.5822659933775,-13.2599708150604));
#11517=CARTESIAN_POINT('Ctrl Pts',(80.9035367880058,-22.6698956607323,-13.371103933052));
#11518=CARTESIAN_POINT('Ctrl Pts',(82.1402511863244,-21.0596498121656,-13.4822370510435));
#11519=CARTESIAN_POINT('Ctrl Pts',(84.1638415383007,-21.2252888269431,-13.5933701690351));
#11520=CARTESIAN_POINT('Ctrl Pts',(85.1222383060715,-23.0152133592554,-13.7045032870266));
#11521=CARTESIAN_POINT('Ctrl Pts',(84.1382790456319,-24.7912140263811,-13.8156364050182));
#11522=CARTESIAN_POINT('Ctrl Pts',(82.1125220004198,-24.9278251150738,-13.9267695230098));
#11523=CARTESIAN_POINT('Ctrl Pts',(80.899019751184,-23.3000147799777,-14.0379026410013));
#11524=CARTESIAN_POINT('Ctrl Pts',(81.6084173195078,-21.3976191098115,-14.1490357589929));
#11525=CARTESIAN_POINT('Ctrl Pts',(83.5914461290462,-20.9617854993789,-14.2601688769844));
#11526=CARTESIAN_POINT('Ctrl Pts',(85.0331601624529,-22.3914060233836,-14.371301994976));
#11527=CARTESIAN_POINT('Ctrl Pts',(84.6140459902515,-24.3780357085581,-14.4824351129676));
#11528=CARTESIAN_POINT('Ctrl Pts',(82.7176934005918,-25.1034328748119,-14.5935682309591));
#11529=CARTESIAN_POINT('Ctrl Pts',(81.0797189200944,-23.9036854827123,-14.7047013489507));
#11530=CARTESIAN_POINT('Ctrl Pts',(81.1992612696318,-21.8768495701431,-14.8158344669422));
#11531=CARTESIAN_POINT('Ctrl Pts',(82.9669105732559,-20.8779651337157,-14.9269675849338));
#11532=CARTESIAN_POINT('Ctrl Pts',(84.7648446392386,-21.8212505374333,-15.0381007029253));
#11533=CARTESIAN_POINT('Ctrl Pts',(84.9475233946487,-23.8433738283793,-15.1492338209169));
#11534=CARTESIAN_POINT('Ctrl Pts',(83.3477521515752,-25.0936082287072,-15.2603669389085));
#11535=CARTESIAN_POINT('Ctrl Pts',(81.4297043202302,-24.4276899107226,-15.3715000569));
#11536=CARTESIAN_POINT('Ctrl Pts',(80.9488531639916,-22.4550937203094,-15.4826331748916));
#11537=CARTESIAN_POINT('Ctrl Pts',(82.345291800469,-20.9812169507322,-15.5937662928831));
#11538=CARTESIAN_POINT('Ctrl Pts',(84.3409461950547,-21.3550103921638,-15.7048994108747));
#11539=CARTESIAN_POINT('Ctrl Pts',(85.1093117692511,-23.2343620602251,-15.8160325288663));
#11540=CARTESIAN_POINT('Ctrl Pts',(83.9471563454166,-24.8992183577035,-15.9271656468579));
#11541=CARTESIAN_POINT('Ctrl Pts',(81.9181178691043,-24.8258312508155,-16.0382987648494));
#11542=CARTESIAN_POINT('Ctrl Pts',(80.8792770238047,-23.0813795174491,-16.149431882841));
#11543=CARTESIAN_POINT('Ctrl Pts',(81.7813723692392,-21.2624300969265,-16.2605650008325));
#11544=CARTESIAN_POINT('Ctrl Pts',(83.7988693899422,-21.0338048477948,-16.3716981188241));
#11545=CARTESIAN_POINT('Ctrl Pts',(85.0850786804704,-22.6046553649229,-16.4828312368156));
#11546=CARTESIAN_POINT('Ctrl Pts',(84.4632031751732,-24.5374673327142,-16.5939643548072));
#11547=CARTESIAN_POINT('Ctrl Pts',(82.5016254341118,-25.0628764630049,-16.7050974727987));
#11548=CARTESIAN_POINT('Ctrl Pts',(80.997219734115,-23.7007628417706,-16.8162305907903));
#11549=CARTESIAN_POINT('Ctrl Pts',(81.3237519397594,-21.696280307798,-16.9273637087819));
#11550=CARTESIAN_POINT('Ctrl Pts',(83.1887491753573,-20.8870198874251,-17.0384968267734));
#11551=CARTESIAN_POINT('Ctrl Pts',(84.3096484764695,-21.6342008454597,-17.1125855721011));
#11552=CARTESIAN_POINT('Ctrl Pts',(84.5881947811615,-22.162290716277,-17.149629944765));
#11553=CARTESIAN_POINT('Ctrl Pts',(84.4664903694652,-21.752733913429,-5.85037005523502));
#11554=CARTESIAN_POINT('Ctrl Pts',(84.8812182065951,-22.2403559097684,-5.88741442789887));
#11555=CARTESIAN_POINT('Ctrl Pts',(85.1785118249911,-23.6537516509257,-5.96150317322658));
#11556=CARTESIAN_POINT('Ctrl Pts',(83.6300848875513,-25.1878876651001,-6.07263629121814));
#11557=CARTESIAN_POINT('Ctrl Pts',(81.5046935938781,-24.7145063291189,-6.1837694092097));
#11558=CARTESIAN_POINT('Ctrl Pts',(80.7480335121834,-22.6744168003776,-6.29490252720125));
#11559=CARTESIAN_POINT('Ctrl Pts',(82.0523753725455,-20.931078211551,-6.40603564519282));
#11560=CARTESIAN_POINT('Ctrl Pts',(84.2240640954254,-21.0819174582576,-6.51716876318437));
#11561=CARTESIAN_POINT('Ctrl Pts',(85.2754193499133,-22.9879508757435,-6.62830188117594));
#11562=CARTESIAN_POINT('Ctrl Pts',(84.2442322035796,-24.9051678125258,-6.73943499916749));
#11563=CARTESIAN_POINT('Ctrl Pts',(82.0742692819441,-25.0786221088941,-6.85056811715905));
#11564=CARTESIAN_POINT('Ctrl Pts',(80.7515743029904,-23.3496787879405,-6.96170123515061));
#11565=CARTESIAN_POINT('Ctrl Pts',(81.4867256385136,-21.3006760442876,-7.07283435314217));
#11566=CARTESIAN_POINT('Ctrl Pts',(83.606885923895,-20.8069713148532,-7.18396747113373));
#11567=CARTESIAN_POINT('Ctrl Pts',(85.1715999777499,-22.3204078177676,-7.29510058912529));
#11568=CARTESIAN_POINT('Ctrl Pts',(84.7487804327262,-24.4558363101326,-7.40623370711685));
#11569=CARTESIAN_POINT('Ctrl Pts',(82.7254081170385,-25.2588248687773,-7.51736682510841));
#11570=CARTESIAN_POINT('Ctrl Pts',(80.9533531442496,-23.9944486236241,-7.62849994309997));
#11571=CARTESIAN_POINT('Ctrl Pts',(81.0544699071237,-21.8199135448055,-7.73963306109153));
#11572=CARTESIAN_POINT('Ctrl Pts',(82.9362123973263,-20.7254401940938,-7.85076617908308));
#11573=CARTESIAN_POINT('Ctrl Pts',(84.8763358066303,-21.7127334250377,-7.96189929707464));
#11574=CARTESIAN_POINT('Ctrl Pts',(85.0991628366174,-23.8781837310767,-8.0730324150662));
#11575=CARTESIAN_POINT('Ctrl Pts',(83.4007534148994,-25.2398857017161,-8.18416553305776));
#11576=CARTESIAN_POINT('Ctrl Pts',(81.3355586950615,-24.5515561270035,-8.29529865104933));
#11577=CARTESIAN_POINT('Ctrl Pts',(80.7937261689251,-22.4431813112383,-8.40643176904087));
#11578=CARTESIAN_POINT('Ctrl Pts',(82.2711622912557,-20.8444288780876,-8.51756488703244));
#11579=CARTESIAN_POINT('Ctrl Pts',(84.4156593713139,-21.2185399769152,-8.628698005024));
#11580=CARTESIAN_POINT('Ctrl Pts',(85.2644892749797,-23.2231134070794,-8.73983112301555));
#11581=CARTESIAN_POINT('Ctrl Pts',(84.0407694647329,-25.0234846651124,-8.85096424100712));
#11582=CARTESIAN_POINT('Ctrl Pts',(81.8644964760864,-24.9718831142117,-8.96209735899868));
#11583=CARTESIAN_POINT('Ctrl Pts',(80.7274810055036,-23.1155365245424,-9.07323047699023));
#11584=CARTESIAN_POINT('Ctrl Pts',(81.6703643641624,-21.1534463601782,-9.1843635949818));
#11585=CARTESIAN_POINT('Ctrl Pts',(83.8301825906873,-20.8813947666021,-9.29549671297334));
#11586=CARTESIAN_POINT('Ctrl Pts',(85.2301850345473,-22.5483740701311,-9.40662983096492));
#11587=CARTESIAN_POINT('Ctrl Pts',(84.5890343555619,-24.6286992004945,-9.51776294895647));
#11588=CARTESIAN_POINT('Ctrl Pts',(82.4935368905835,-25.218374717592,-9.62889606694802));
#11589=CARTESIAN_POINT('Ctrl Pts',(80.8615743975369,-23.77770637877,-9.7400291849396));
#11590=CARTESIAN_POINT('Ctrl Pts',(81.186783183476,-21.6252505518735,-9.85116230293115));
#11591=CARTESIAN_POINT('Ctrl Pts',(83.1715193674164,-20.7310195295131,-9.96229542092271));
#11592=CARTESIAN_POINT('Ctrl Pts',(84.9992742753607,-21.9134487399435,-10.0734285389143));
#11593=CARTESIAN_POINT('Ctrl Pts',(84.9972146758263,-24.0903324298184,-10.1845616569058));
#11594=CARTESIAN_POINT('Ctrl Pts',(83.167225595372,-25.2693009648573,-10.2956947748974));
#11595=CARTESIAN_POINT('Ctrl Pts',(81.1841850680979,-24.3713159380432,-10.4068278928889));
#11596=CARTESIAN_POINT('Ctrl Pts',(80.8630498362799,-22.2182485902626,-10.5179610108805));
#11597=CARTESIAN_POINT('Ctrl Pts',(82.4977355038374,-20.7806709021093,-10.6290941288721));
#11598=CARTESIAN_POINT('Ctrl Pts',(84.5921134072207,-21.3743105562877,-10.7402272468636));
#11599=CARTESIAN_POINT('Ctrl Pts',(85.2293264553427,-23.4558451758645,-10.8513603648552));
#11600=CARTESIAN_POINT('Ctrl Pts',(83.8261721861007,-25.1201723485988,-10.9624934828468));
#11601=CARTESIAN_POINT('Ctrl Pts',(81.666872614319,-24.8440343387251,-11.0736266008383));
#11602=CARTESIAN_POINT('Ctrl Pts',(80.7277036972952,-22.8801635215658,-11.1847597188299));
#11603=CARTESIAN_POINT('Ctrl Pts',(81.8682297932177,-21.0259717661873,-11.2958928368214));
#11604=CARTESIAN_POINT('Ctrl Pts',(84.0445965284286,-20.9784883473884,-11.407025954813));
#11605=CARTESIAN_POINT('Ctrl Pts',(85.264907405903,-22.7811719589829,-11.5181590728045));
#11606=CARTESIAN_POINT('Ctrl Pts',(84.4122858796081,-24.784135606704,-11.6292921907961));
#11607=CARTESIAN_POINT('Ctrl Pts',(82.2670847292654,-25.1541881242764,-11.7404253087876));
#11608=CARTESIAN_POINT('Ctrl Pts',(80.7926764819628,-23.5526428824927,-11.8515584267792));
#11609=CARTESIAN_POINT('Ctrl Pts',(81.3384975977751,-21.4452971228397,-11.9626915447708));
#11610=CARTESIAN_POINT('Ctrl Pts',(83.4049911082007,-20.7608766288728,-12.0738246627623));
#11611=CARTESIAN_POINT('Ctrl Pts',(85.1008208161065,-22.1257899751985,-12.1849577807539));
#11612=CARTESIAN_POINT('Ctrl Pts',(84.87389662561,-24.2908147447938,-12.2960908987455));
#11613=CARTESIAN_POINT('Ctrl Pts',(82.9319084875028,-25.2744350539806,-12.407224016737));
#11614=CARTESIAN_POINT('Ctrl Pts',(81.0522403816889,-24.1764028808729,-12.5183571347286));
#11615=CARTESIAN_POINT('Ctrl Pts',(80.9552385416248,-22.0016804884241,-12.6294902527201));
#11616=CARTESIAN_POINT('Ctrl Pts',(82.7296828692925,-20.7406594064427,-12.7406233707117));
#11617=CARTESIAN_POINT('Ctrl Pts',(84.7515320745623,-21.5474757624641,-12.8517564887033));
#11618=CARTESIAN_POINT('Ctrl Pts',(85.170310185562,-23.6836994714752,-12.9628896066948));
#11619=CARTESIAN_POINT('Ctrl Pts',(83.6027349921588,-25.1941745140432,-13.0740227246864));
#11620=CARTESIAN_POINT('Ctrl Pts',(81.483513010514,-24.6964546794916,-13.1851558426779));
#11621=CARTESIAN_POINT('Ctrl Pts',(80.7522396099925,-22.6460727504636,-13.2962889606695));
#11622=CARTESIAN_POINT('Ctrl Pts',(82.0782049893937,-20.9196189706525,-13.407422078661));
#11623=CARTESIAN_POINT('Ctrl Pts',(84.2478334439978,-21.0972117918987,-13.5185551966526));
#11624=CARTESIAN_POINT('Ctrl Pts',(85.2753956164136,-23.0163112742153,-13.6296883146442));
#11625=CARTESIAN_POINT('Ctrl Pts',(84.2204261619801,-24.9204820363604,-13.7408214326357));
#11626=CARTESIAN_POINT('Ctrl Pts',(82.0484746486146,-25.0669520494006,-13.8519545506273));
#11627=CARTESIAN_POINT('Ctrl Pts',(80.747396588474,-23.3216661923723,-13.9630876686188));
#11628=CARTESIAN_POINT('Ctrl Pts',(81.5079898322398,-21.2819787754613,-14.0742207866104));
#11629=CARTESIAN_POINT('Ctrl Pts',(83.6341295063454,-20.8146920038359,-14.1853539046019));
#11630=CARTESIAN_POINT('Ctrl Pts',(85.1798888974328,-22.3474851233215,-14.2964870225935));
#11631=CARTESIAN_POINT('Ctrl Pts',(84.730528169434,-24.4774855404051,-14.4076201405851));
#11632=CARTESIAN_POINT('Ctrl Pts',(82.6973199489705,-25.2552330381911,-14.5187532585766));
#11633=CARTESIAN_POINT('Ctrl Pts',(80.9411364223337,-23.9689024932297,-14.6298863765682));
#11634=CARTESIAN_POINT('Ctrl Pts',(81.0693058825373,-21.7957942530026,-14.7410194945597));
#11635=CARTESIAN_POINT('Ctrl Pts',(82.9645225814897,-20.7248225051793,-14.8521526125513));
#11636=CARTESIAN_POINT('Ctrl Pts',(84.8922096280545,-21.7361827593532,-14.9632857305429));
#11637=CARTESIAN_POINT('Ctrl Pts',(85.0880719108542,-23.9042382783319,-15.0744188485344));
#11638=CARTESIAN_POINT('Ctrl Pts',(83.3728486659716,-25.2446993688028,-15.185551966526));
#11639=CARTESIAN_POINT('Ctrl Pts',(81.3163795055442,-24.5307231780532,-15.2966850845175));
#11640=CARTESIAN_POINT('Ctrl Pts',(80.8008263700066,-22.4157690224434,-15.4078182025091));
#11641=CARTESIAN_POINT('Ctrl Pts',(82.2980429375056,-20.8355257806569,-15.5189513205006));
#11642=CARTESIAN_POINT('Ctrl Pts',(84.4377193575977,-21.2362950795827,-15.6300844384922));
#11643=CARTESIAN_POINT('Ctrl Pts',(85.2615361996211,-23.2512754590115,-15.7412175564838));
#11644=CARTESIAN_POINT('Ctrl Pts',(84.0155105532936,-25.0362808047369,-15.8523506744753));
#11645=CARTESIAN_POINT('Ctrl Pts',(81.8400407951012,-24.9575975103884,-15.9634837924669));
#11646=CARTESIAN_POINT('Ctrl Pts',(80.7262290715151,-23.0872524997498,-16.0746169104584));
#11647=CARTESIAN_POINT('Ctrl Pts',(81.6934266707275,-21.1370334663385,-16.18575002845));
#11648=CARTESIAN_POINT('Ctrl Pts',(83.8565220516287,-20.8919088315662,-16.2968831464416));
#11649=CARTESIAN_POINT('Ctrl Pts',(85.2355542616711,-22.5761242047825,-16.4080162644331));
#11650=CARTESIAN_POINT('Ctrl Pts',(84.5687993573514,-24.6484229971859,-16.5191493824247));
#11651=CARTESIAN_POINT('Ctrl Pts',(82.4656588285538,-25.2117497585901,-16.6302825004162));
#11652=CARTESIAN_POINT('Ctrl Pts',(80.8526834500174,-23.7513353678277,-16.7414156184078));
#11653=CARTESIAN_POINT('Ctrl Pts',(81.2027807728371,-21.6021937007821,-16.8525487363994));
#11654=CARTESIAN_POINT('Ctrl Pts',(83.2023707917161,-20.7345307207171,-16.9636818543909));
#11655=CARTESIAN_POINT('Ctrl Pts',(84.4041629509165,-21.5356340990305,-17.0377705997186));
#11656=CARTESIAN_POINT('Ctrl Pts',(84.7028113349605,-22.1018350641589,-17.0748149723825));
#11657=CARTESIAN_POINT('Ctrl Pts',(84.5652001142717,-21.6687801966678,-5.77555508285253));
#11658=CARTESIAN_POINT('Ctrl Pts',(85.0078433607487,-22.1892241220309,-5.81259945551639));
#11659=CARTESIAN_POINT('Ctrl Pts',(85.325147868964,-23.6977557984969,-5.88668820084409));
#11660=CARTESIAN_POINT('Ctrl Pts',(83.6724960207927,-25.3351547986483,-5.99782131883565));
#11661=CARTESIAN_POINT('Ctrl Pts',(81.4040442361811,-24.829910075192,-6.10895443682721));
#11662=CARTESIAN_POINT('Ctrl Pts',(80.5964532209291,-22.6525017334824,-6.22008755481877));
#11663=CARTESIAN_POINT('Ctrl Pts',(81.9885905792076,-20.7918186937154,-6.33122067281033));
#11664=CARTESIAN_POINT('Ctrl Pts',(84.3064560817636,-20.952810958716,-6.44235379080188));
#11665=CARTESIAN_POINT('Ctrl Pts',(85.4285782577618,-22.9871398469054,-6.55348690879345));
#11666=CARTESIAN_POINT('Ctrl Pts',(84.3279817091015,-25.0334050191953,-6.664620026785));
#11667=CARTESIAN_POINT('Ctrl Pts',(82.0119581717988,-25.218534557138,-6.77575314477657));
#11668=CARTESIAN_POINT('Ctrl Pts',(80.6002323430368,-23.3732157334538,-6.88688626276812));
#11669=CARTESIAN_POINT('Ctrl Pts',(81.3848668543341,-21.186294226647,-6.99801938075968));
#11670=CARTESIAN_POINT('Ctrl Pts',(83.6477355304943,-20.659358138271,-7.10915249875124));
#11671=CARTESIAN_POINT('Ctrl Pts',(85.3177707839745,-22.2746643391349,-7.2202856167428));
#11672=CARTESIAN_POINT('Ctrl Pts',(84.8664911752114,-24.5538289281854,-7.33141873473436));
#11673=CARTESIAN_POINT('Ctrl Pts',(82.7069252853353,-25.4108667989543,-7.44255185272592));
#11674=CARTESIAN_POINT('Ctrl Pts',(80.8155929563571,-24.0613851490217,-7.55368497071747));
#11675=CARTESIAN_POINT('Ctrl Pts',(80.9235159077116,-21.7404817017691,-7.66481808870904));
#11676=CARTESIAN_POINT('Ctrl Pts',(82.9319188416964,-20.5723391423155,-7.77595120670059));
#11677=CARTESIAN_POINT('Ctrl Pts',(85.0026323255168,-21.6260872678191,-7.88708432469216));
#11678=CARTESIAN_POINT('Ctrl Pts',(85.2404578851386,-23.9372944445138,-7.99821744268371));
#11679=CARTESIAN_POINT('Ctrl Pts',(83.4277282032368,-25.3906528329675,-8.10935056067527));
#11680=CARTESIAN_POINT('Ctrl Pts',(81.2235248352579,-24.6559916640778,-8.22048367866684));
#11681=CARTESIAN_POINT('Ctrl Pts',(80.6452214590593,-22.4057017397283,-8.33161679665839));
#11682=CARTESIAN_POINT('Ctrl Pts',(82.2221040868968,-20.6993369771883,-8.44274991464995));
#11683=CARTESIAN_POINT('Ctrl Pts',(84.5109476719975,-21.0986295650073,-8.55388303264151));
#11684=CARTESIAN_POINT('Ctrl Pts',(85.4169124774121,-23.2381312128108,-8.66501615063307));
#11685=CARTESIAN_POINT('Ctrl Pts',(84.1108238547277,-25.1596858015617,-8.77614926862463));
#11686=CARTESIAN_POINT('Ctrl Pts',(81.7880655186073,-25.1046109404864,-8.88728238661618));
#11687=CARTESIAN_POINT('Ctrl Pts',(80.5745173211281,-23.1233133099144,-8.99841550460776));
#11688=CARTESIAN_POINT('Ctrl Pts',(81.5808663374233,-21.0291544845863,-9.10954862259929));
#11689=CARTESIAN_POINT('Ctrl Pts',(83.886062338264,-20.7387910466673,-9.22068174059087));
#11690=CARTESIAN_POINT('Ctrl Pts',(85.3802992120524,-22.517975043166,-9.33181485858242));
#11691=CARTESIAN_POINT('Ctrl Pts',(84.695992559306,-24.7383272524714,-9.44294797657398));
#11692=CARTESIAN_POINT('Ctrl Pts',(82.4594467626664,-25.3676939404236,-9.55408109456554));
#11693=CARTESIAN_POINT('Ctrl Pts',(80.7176365648024,-23.8300539425735,-9.6652142125571));
#11694=CARTESIAN_POINT('Ctrl Pts',(81.0647352157808,-21.5327159058759,-9.77634733054867));
#11695=CARTESIAN_POINT('Ctrl Pts',(83.1830643685562,-20.5782940238596,-9.88748044854021));
#11696=CARTESIAN_POINT('Ctrl Pts',(85.1338458058857,-21.8403127686255,-9.99861356653179));
#11697=CARTESIAN_POINT('Ctrl Pts',(85.131647574316,-24.1637229123899,-10.1097466845233));
#11698=CARTESIAN_POINT('Ctrl Pts',(83.1784815819015,-25.4220480430476,-10.2208798025149));
#11699=CARTESIAN_POINT('Ctrl Pts',(81.061962220764,-24.4636194738261,-10.3320129205064));
#11700=CARTESIAN_POINT('Ctrl Pts',(80.7192113156071,-22.1656287546578,-10.443146038498));
#11701=CARTESIAN_POINT('Ctrl Pts',(82.4639279853743,-20.6312874397589,-10.5542791564896));
#11702=CARTESIAN_POINT('Ctrl Pts',(84.699278862516,-21.2648850916105,-10.6654122744811));
#11703=CARTESIAN_POINT('Ctrl Pts',(85.3793828417187,-23.4865282010775,-10.7765453924727));
#11704=CARTESIAN_POINT('Ctrl Pts',(83.8817819925845,-25.2628815513549,-10.8876785104643));
#11705=CARTESIAN_POINT('Ctrl Pts',(81.577139557236,-24.9681566396824,-10.9988116284558));
#11706=CARTESIAN_POINT('Ctrl Pts',(80.5747550023464,-22.8720973054821,-11.1099447464474));
#11707=CARTESIAN_POINT('Ctrl Pts',(81.7920501260224,-20.8930995515055,-11.2210778644389));
#11708=CARTESIAN_POINT('Ctrl Pts',(84.1149085188063,-20.8424200147847,-11.3322109824305));
#11709=CARTESIAN_POINT('Ctrl Pts',(85.4173587528071,-22.7664426020535,-11.443344100422));
#11710=CARTESIAN_POINT('Ctrl Pts',(84.5073471099255,-24.9042261126527,-11.5544772184136));
#11711=CARTESIAN_POINT('Ctrl Pts',(82.2177520634359,-25.2991869353425,-11.6656103364051));
#11712=CARTESIAN_POINT('Ctrl Pts',(80.6441011174686,-23.5898413796911,-11.7767434543967));
#11713=CARTESIAN_POINT('Ctrl Pts',(81.2266615560704,-21.3406497774158,-11.8878765723883));
#11714=CARTESIAN_POINT('Ctrl Pts',(83.4322511364777,-20.6101608102379,-11.9990096903798));
#11715=CARTESIAN_POINT('Ctrl Pts',(85.2422274635415,-22.0669467326842,-12.1101428083714));
#11716=CARTESIAN_POINT('Ctrl Pts',(85.0000289627594,-24.3776997299966,-12.221275926363));
#11717=CARTESIAN_POINT('Ctrl Pts',(82.9273252348868,-25.4275277086832,-12.3324090443545));
#11718=CARTESIAN_POINT('Ctrl Pts',(80.9211363124968,-24.2555867818233,-12.4435421623461));
#11719=CARTESIAN_POINT('Ctrl Pts',(80.8176052601872,-21.9344834128246,-12.5546752803376));
#11720=CARTESIAN_POINT('Ctrl Pts',(82.711487771974,-20.588582762733,-12.6658083983292));
#11721=CARTESIAN_POINT('Ctrl Pts',(84.869428030581,-21.4497060806457,-12.7769415163207));
#11722=CARTESIAN_POINT('Ctrl Pts',(85.3163941756299,-23.7297194125255,-12.8880746343123));
#11723=CARTESIAN_POINT('Ctrl Pts',(83.6433051987559,-25.3418648165858,-12.9992077523039));
#11724=CARTESIAN_POINT('Ctrl Pts',(81.3814379837349,-24.8106433656058,-13.1103408702954));
#11725=CARTESIAN_POINT('Ctrl Pts',(80.6009424319792,-22.6222498401948,-13.221473988287));
#11726=CARTESIAN_POINT('Ctrl Pts',(82.0161587924632,-20.7795881291394,-13.3326071062786));
#11727=CARTESIAN_POINT('Ctrl Pts',(84.3318253496949,-20.9691347568542,-13.4437402242701));
#11728=CARTESIAN_POINT('Ctrl Pts',(85.4285529267558,-23.0174091891753,-13.5548733422617));
#11729=CARTESIAN_POINT('Ctrl Pts',(84.3025732783284,-25.0497500463396,-13.6660064602532));
#11730=CARTESIAN_POINT('Ctrl Pts',(81.9844272968094,-25.2060789837275,-13.7771395782448));
#11731=CARTESIAN_POINT('Ctrl Pts',(80.5957734257642,-23.3433176047668,-13.8882726962363));
#11732=CARTESIAN_POINT('Ctrl Pts',(81.4075623449717,-21.1663384411112,-13.9994058142279));
#11733=CARTESIAN_POINT('Ctrl Pts',(83.6768128836446,-20.6675985082928,-14.1105389322194));
#11734=CARTESIAN_POINT('Ctrl Pts',(85.326617632413,-22.3035642232594,-14.221672050211));
#11735=CARTESIAN_POINT('Ctrl Pts',(84.8470103486162,-24.5769353722521,-14.3328051682026));
#11736=CARTESIAN_POINT('Ctrl Pts',(82.6769464973495,-25.4070332015704,-14.4439382861941));
#11737=CARTESIAN_POINT('Ctrl Pts',(80.8025539245727,-24.0341195037471,-14.5550714041857));
#11738=CARTESIAN_POINT('Ctrl Pts',(80.9393504954431,-21.714738935862,-14.6662045221772));
#11739=CARTESIAN_POINT('Ctrl Pts',(82.9621345897233,-20.571679876643,-14.7773376401688));
#11740=CARTESIAN_POINT('Ctrl Pts',(85.0195746168704,-21.6511149812732,-14.8884707581604));
#11741=CARTESIAN_POINT('Ctrl Pts',(85.2286204270596,-23.9651027282846,-14.9996038761519));
#11742=CARTESIAN_POINT('Ctrl Pts',(83.397945180368,-25.3957905088984,-15.1107369941435));
#11743=CARTESIAN_POINT('Ctrl Pts',(81.203054690858,-24.6337564453839,-15.221870112135));
#11744=CARTESIAN_POINT('Ctrl Pts',(80.6527995760217,-22.3764443245774,-15.3330032301266));
#11745=CARTESIAN_POINT('Ctrl Pts',(82.2507940745424,-20.6898346105816,-15.4441363481181));
#11746=CARTESIAN_POINT('Ctrl Pts',(84.5344925201404,-21.1175797670015,-15.5552694661097));
#11747=CARTESIAN_POINT('Ctrl Pts',(85.4137606299914,-23.2681888577979,-15.6664025841013));
#11748=CARTESIAN_POINT('Ctrl Pts',(84.0838647611703,-25.1733432517703,-15.7775357020929));
#11749=CARTESIAN_POINT('Ctrl Pts',(81.7619637210983,-25.0893637699614,-15.8886688200844));
#11750=CARTESIAN_POINT('Ctrl Pts',(80.5731811192254,-23.0931254820504,-15.999801938076));
#11751=CARTESIAN_POINT('Ctrl Pts',(81.6054809722158,-21.0116368357505,-16.1109350560675));
#11752=CARTESIAN_POINT('Ctrl Pts',(83.9141747133152,-20.7500128153374,-16.2220681740591));
#11753=CARTESIAN_POINT('Ctrl Pts',(85.3860298428717,-22.5475930446421,-16.3332012920507));
#11754=CARTESIAN_POINT('Ctrl Pts',(84.6743955395297,-24.7593786616575,-16.4443344100422));
#11755=CARTESIAN_POINT('Ctrl Pts',(82.4296922229958,-25.3606230541752,-16.5554675280338));
#11756=CARTESIAN_POINT('Ctrl Pts',(80.7081471659199,-23.8019078938848,-16.6666006460253));
#11757=CARTESIAN_POINT('Ctrl Pts',(81.0818096059147,-21.508107093766,-16.7777337640169));
#11758=CARTESIAN_POINT('Ctrl Pts',(83.2159924080748,-20.5820415540093,-16.8888668820084));
#11759=CARTESIAN_POINT('Ctrl Pts',(84.4986774253636,-21.4370673526013,-16.9629556273361));
#11760=CARTESIAN_POINT('Ctrl Pts',(84.8174278887595,-22.0413794120407,-17.));
#11761=CARTESIAN_POINT('Ctrl Pts',(84.2690708798524,-21.9206413469515,-6.));
#11762=CARTESIAN_POINT('Ctrl Pts',(84.31440005766,-21.9629286589163,-6.));
#11763=CARTESIAN_POINT('Ctrl Pts',(84.3569992287073,-22.0077850881403,-6.));
#11764=CARTESIAN_POINT('Ctrl Pts',(84.3968698737015,-22.0548656097299,-6.));
#11765=CARTESIAN_POINT('Ctrl Pts',(84.439372145716,-22.1050536399329,-6.));
#11766=CARTESIAN_POINT('Ctrl Pts',(84.4787745414504,-22.1577692838041,-6.));
#11767=CARTESIAN_POINT('Ctrl Pts',(84.5150500219472,-22.2126493042886,-6.));
#11768=CARTESIAN_POINT('Ctrl Pts',(84.5467910673818,-22.2606693222126,-6.));
#11769=CARTESIAN_POINT('Ctrl Pts',(84.5761378249178,-22.3103476665893,-6.));
#11770=CARTESIAN_POINT('Ctrl Pts',(84.6030492875067,-22.3614685512206,-6.));
#11771=CARTESIAN_POINT('Ctrl Pts',(84.6165495358461,-22.3871135579004,-6.));
#11772=CARTESIAN_POINT('Ctrl Pts',(84.6294365646594,-22.4131219455844,-6.));
#11773=CARTESIAN_POINT('Ctrl Pts',(84.6417028557084,-22.4394683134584,-6.));
#11774=CARTESIAN_POINT('Ctrl Pts',(84.6473118270288,-22.4515156406588,-6.));
#11775=CARTESIAN_POINT('Ctrl Pts',(84.6527915844349,-22.4636353215094,-6.));
#11776=CARTESIAN_POINT('Ctrl Pts',(84.6581328964447,-22.4758049682417,-6.));
#11777=CARTESIAN_POINT('Ctrl Pts',(84.6850518037078,-22.5371370138533,-6.));
#11778=CARTESIAN_POINT('Ctrl Pts',(84.7085095493669,-22.5998445222056,-6.));
#11779=CARTESIAN_POINT('Ctrl Pts',(84.7284826296036,-22.6635697254165,-6.));
#11780=CARTESIAN_POINT('Ctrl Pts',(84.7488100298177,-22.7284254058644,-6.));
#11781=CARTESIAN_POINT('Ctrl Pts',(84.7655285903436,-22.7943360504365,-6.));
#11782=CARTESIAN_POINT('Ctrl Pts',(84.7785742179873,-22.8609610235803,-6.));
#11783=CARTESIAN_POINT('Ctrl Pts',(84.7894854413479,-22.9166854381682,-6.));
#11784=CARTESIAN_POINT('Ctrl Pts',(84.7978267202991,-22.9729105003599,-6.));
#11785=CARTESIAN_POINT('Ctrl Pts',(84.8035357299874,-23.0294491921539,-6.));
#11786=CARTESIAN_POINT('Ctrl Pts',(84.8061653446974,-23.0554913577379,-6.));
#11787=CARTESIAN_POINT('Ctrl Pts',(84.8082361631249,-23.0816001759408,-6.));
#11788=CARTESIAN_POINT('Ctrl Pts',(84.8097402930293,-23.1077577720533,-6.));
#11789=CARTESIAN_POINT('Ctrl Pts',(84.8103976576895,-23.1191896831064,-6.));
#11790=CARTESIAN_POINT('Ctrl Pts',(84.810946665569,-23.1306307060492,-6.));
#11791=CARTESIAN_POINT('Ctrl Pts',(84.8113863231945,-23.1420652136516,-6.));
#11792=CARTESIAN_POINT('Ctrl Pts',(84.8140826819691,-23.2121914507941,-6.));
#11793=CARTESIAN_POINT('Ctrl Pts',(84.8126783065445,-23.2822039935574,-6.));
#11794=CARTESIAN_POINT('Ctrl Pts',(84.8071185682592,-23.3517420391025,-6.));
#11795=CARTESIAN_POINT('Ctrl Pts',(84.8021489988479,-23.4138985879056,-6.));
#11796=CARTESIAN_POINT('Ctrl Pts',(84.7938590814259,-23.4756769926154,-6.));
#11797=CARTESIAN_POINT('Ctrl Pts',(84.7821766931341,-23.5368317128957,-6.));
#11798=CARTESIAN_POINT('Ctrl Pts',(84.7694462372846,-23.6034728351621,-6.));
#11799=CARTESIAN_POINT('Ctrl Pts',(84.7526883937327,-23.6693741806892,-6.));
#11800=CARTESIAN_POINT('Ctrl Pts',(84.7321483928848,-23.7343221733006,-6.));
#11801=CARTESIAN_POINT('Ctrl Pts',(84.7242190379921,-23.7593949903273,-6.));
#11802=CARTESIAN_POINT('Ctrl Pts',(84.715725472557,-23.7843256816232,-6.));
#11803=CARTESIAN_POINT('Ctrl Pts',(84.7066797953178,-23.809101639147,-6.));
#11804=CARTESIAN_POINT('Ctrl Pts',(84.7027124228906,-23.8199682053687,-6.));
#11805=CARTESIAN_POINT('Ctrl Pts',(84.698638945642,-23.8308044388952,-6.));
#11806=CARTESIAN_POINT('Ctrl Pts',(84.6944654696784,-23.8415967394888,-6.));
#11807=CARTESIAN_POINT('Ctrl Pts',(84.6692426561464,-23.9068210723529,-6.));
#11808=CARTESIAN_POINT('Ctrl Pts',(84.6403290249097,-23.9705599886322,-6.));
#11809=CARTESIAN_POINT('Ctrl Pts',(84.6080372321188,-24.0325946845425,-6.));
#11810=CARTESIAN_POINT('Ctrl Pts',(84.5749974356073,-24.0960663456795,-6.));
#11811=CARTESIAN_POINT('Ctrl Pts',(84.5384208599741,-24.1577547385726,-6.));
#11812=CARTESIAN_POINT('Ctrl Pts',(84.4985862577967,-24.2174217857006,-6.));
#11813=CARTESIAN_POINT('Ctrl Pts',(84.4680936319117,-24.2630957687779,-6.));
#11814=CARTESIAN_POINT('Ctrl Pts',(84.4356907141024,-24.3075853544397,-6.));
#11815=CARTESIAN_POINT('Ctrl Pts',(84.4014829883928,-24.3507776514475,-6.));
#11816=CARTESIAN_POINT('Ctrl Pts',(84.3801864571408,-24.3776676619347,-6.));
#11817=CARTESIAN_POINT('Ctrl Pts',(84.3581900818954,-24.4040547371998,-6.));
#11818=CARTESIAN_POINT('Ctrl Pts',(84.3355164080287,-24.4299099472039,-6.));
#11819=CARTESIAN_POINT('Ctrl Pts',(84.3228383139497,-24.444367012556,-6.));
#11820=CARTESIAN_POINT('Ctrl Pts',(84.3099439935595,-24.458662320114,-6.));
#11821=CARTESIAN_POINT('Ctrl Pts',(84.2968610717558,-24.4727654072714,-6.));
#11822=CARTESIAN_POINT('Ctrl Pts',(84.2459898547062,-24.5276034028369,-6.));
#11823=CARTESIAN_POINT('Ctrl Pts',(84.192222096132,-24.5795964550668,-6.));
#11824=CARTESIAN_POINT('Ctrl Pts',(84.135842741352,-24.6284806457894,-6.));
#11825=CARTESIAN_POINT('Ctrl Pts',(84.0936831880685,-24.66503543879,-6.));
#11826=CARTESIAN_POINT('Ctrl Pts',(84.0500621252999,-24.6998516194455,-6.));
#11827=CARTESIAN_POINT('Ctrl Pts',(84.0050823134671,-24.7328090870297,-6.));
#11828=CARTESIAN_POINT('Ctrl Pts',(83.9910186700033,-24.7431137560509,-6.));
#11829=CARTESIAN_POINT('Ctrl Pts',(83.9768221028881,-24.7532366406933,-6.));
#11830=CARTESIAN_POINT('Ctrl Pts',(83.9624955117011,-24.7631738431009,-6.));
#11831=CARTESIAN_POINT('Ctrl Pts',(83.9487061657523,-24.7727384017579,-6.));
#11832=CARTESIAN_POINT('Ctrl Pts',(83.9348034056216,-24.782125996426,-6.));
#11833=CARTESIAN_POINT('Ctrl Pts',(83.9207951905357,-24.7913304106764,-6.));
#11834=CARTESIAN_POINT('Ctrl Pts',(83.8578415187256,-24.8326955432339,-6.));
#11835=CARTESIAN_POINT('Ctrl Pts',(83.7927303913155,-24.8703850018091,-6.));
#11836=CARTESIAN_POINT('Ctrl Pts',(83.7257230914976,-24.9041196200216,-6.));
#11837=CARTESIAN_POINT('Ctrl Pts',(83.6744957034376,-24.929909890379,-6.));
#11838=CARTESIAN_POINT('Ctrl Pts',(83.6221590906546,-24.9533882784112,-6.));
#11839=CARTESIAN_POINT('Ctrl Pts',(83.5688161346424,-24.9744147904526,-6.));
#11840=CARTESIAN_POINT('Ctrl Pts',(83.5563688919884,-24.9793211945425,-6.));
#11841=CARTESIAN_POINT('Ctrl Pts',(83.5438668104282,-24.9840940285375,-6.));
#11842=CARTESIAN_POINT('Ctrl Pts',(83.5313118283826,-24.9887338811667,-6.));
#11843=CARTESIAN_POINT('Ctrl Pts',(81.3326823670782,-23.0013023207031,-7.12851963660979));
#11844=CARTESIAN_POINT('Ctrl Pts',(81.3319480813151,-23.0867862355622,-7.12279015104505));
#11845=CARTESIAN_POINT('Ctrl Pts',(81.3379547004357,-23.1721666229398,-7.11706066548032));
#11846=CARTESIAN_POINT('Ctrl Pts',(81.351061266783,-23.2564427466052,-7.11133117991559));
#11847=CARTESIAN_POINT('Ctrl Pts',(81.4358026493434,-23.8013356687448,-7.07428680725173));
#11848=CARTESIAN_POINT('Ctrl Pts',(81.8173470757891,-24.3000664405756,-7.03724243458788));
#11849=CARTESIAN_POINT('Ctrl Pts',(82.3210929040621,-24.5244145242877,-7.00019806192403));
#11850=CARTESIAN_POINT('Ctrl Pts',(82.8248387323351,-24.7487626079999,-6.96315368926018));
#11851=CARTESIAN_POINT('Ctrl Pts',(83.4507859624355,-24.6987280035934,-6.92610931659633));
#11852=CARTESIAN_POINT('Ctrl Pts',(83.9124876344324,-24.3971906237623,-6.88906494393247));
#11853=CARTESIAN_POINT('Ctrl Pts',(84.3741893064293,-24.0956532439312,-6.85202057126862));
#11854=CARTESIAN_POINT('Ctrl Pts',(84.6716454203228,-23.5426130886755,-6.81497619860477));
#11855=CARTESIAN_POINT('Ctrl Pts',(84.6687365753584,-22.9911859317011,-6.77793182594091));
#11856=CARTESIAN_POINT('Ctrl Pts',(84.6658277303939,-22.4397587747268,-6.74088745327706));
#11857=CARTESIAN_POINT('Ctrl Pts',(84.3625539265714,-21.8899446160338,-6.70384308061321));
#11858=CARTESIAN_POINT('Ctrl Pts',(83.8976944974056,-21.5932820016675,-6.66679870794935));
#11859=CARTESIAN_POINT('Ctrl Pts',(83.4328350682397,-21.2966193873012,-6.6297543352855));
#11860=CARTESIAN_POINT('Ctrl Pts',(82.8063900137305,-21.2531083172617,-6.59270996262165));
#11861=CARTESIAN_POINT('Ctrl Pts',(82.3050423423877,-21.4827943967329,-6.5556655899578));
#11862=CARTESIAN_POINT('Ctrl Pts',(81.8036946710448,-21.7124804762041,-6.51862121729394));
#11863=CARTESIAN_POINT('Ctrl Pts',(81.4274443828683,-22.215363705186,-6.48157684463009));
#11864=CARTESIAN_POINT('Ctrl Pts',(81.3484522745435,-22.7610473034778,-6.44453247196624));
#11865=CARTESIAN_POINT('Ctrl Pts',(81.3370705402061,-22.8396732052259,-6.43919486018076));
#11866=CARTESIAN_POINT('Ctrl Pts',(81.3318602001293,-22.919187687916,-6.43385724839527));
#11867=CARTESIAN_POINT('Ctrl Pts',(81.3325225746862,-22.9987867636662,-6.42851963660979));
#11868=CARTESIAN_POINT('Ctrl Pts',(82.4698297828114,-24.9851743256717,-6.));
#11869=CARTESIAN_POINT('Ctrl Pts',(81.8097404375819,-24.8088876857537,-6.03704437266385));
#11870=CARTESIAN_POINT('Ctrl Pts',(80.6907280394499,-23.748620932819,-6.11113311799156));
#11871=CARTESIAN_POINT('Ctrl Pts',(81.1186741085106,-21.4618810792727,-6.22226623598312));
#11872=CARTESIAN_POINT('Ctrl Pts',(83.2718171975381,-20.587166548819,-6.33339935397468));
#11873=CARTESIAN_POINT('Ctrl Pts',(85.1745320976991,-21.9187032679059,-6.44453247196624));
#11874=CARTESIAN_POINT('Ctrl Pts',(85.0878555654783,-24.2409162559102,-6.55566558995779));
#11875=CARTESIAN_POINT('Ctrl Pts',(83.0898774551597,-25.4268774336938,-6.66679870794935));
#11876=CARTESIAN_POINT('Ctrl Pts',(81.0098475173314,-24.3919237452049,-6.77793182594092));
#11877=CARTESIAN_POINT('Ctrl Pts',(80.751179398391,-22.0828968633224,-6.88906494393247));
#11878=CARTESIAN_POINT('Ctrl Pts',(82.550772583103,-20.6133039463769,-7.00019806192403));
#11879=CARTESIAN_POINT('Ctrl Pts',(84.7614902208339,-21.3280765684321,-7.11133117991559));
#11880=CARTESIAN_POINT('Ctrl Pts',(85.3600357932379,-23.5730756808161,-7.22246429790715));
#11881=CARTESIAN_POINT('Ctrl Pts',(83.7985771412431,-25.2935651717014,-7.33359741589871));
#11882=CARTESIAN_POINT('Ctrl Pts',(81.5062325551516,-24.9148976561351,-7.44473053389026));
#11883=CARTESIAN_POINT('Ctrl Pts',(80.5810410755085,-22.7836383740802,-7.55586365188183));
#11884=CARTESIAN_POINT('Ctrl Pts',(81.8697768417376,-20.8504028018083,-7.66699676987338));
#11885=CARTESIAN_POINT('Ctrl Pts',(84.192936911971,-20.8845626742973,-7.77812988786495));
#11886=CARTESIAN_POINT('Ctrl Pts',(85.4242743751978,-22.854854309961,-7.8892630058565));
#11887=CARTESIAN_POINT('Ctrl Pts',(84.4368204072615,-24.9579888637226,-8.00039612384806));
#11888=CARTESIAN_POINT('Ctrl Pts',(82.1343319022801,-25.2690950090472,-8.11152924183961));
#11889=CARTESIAN_POINT('Ctrl Pts',(80.6241368864335,-23.5034360586258,-8.22266235983119));
#11890=CARTESIAN_POINT('Ctrl Pts',(81.2884253183515,-21.2770126287236,-8.33379547782273));
#11891=CARTESIAN_POINT('Ctrl Pts',(83.5192142592352,-20.6275350489011,-8.44492859581431));
#11892=CARTESIAN_POINT('Ctrl Pts',(85.2747978773029,-22.1494307757635,-8.55606171380584));
#11893=CARTESIAN_POINT('Ctrl Pts',(84.9483969412313,-24.4498009326555,-8.66719483179743));
#11894=CARTESIAN_POINT('Ctrl Pts',(82.8387464372207,-25.4232562134105,-8.77832794978897));
#11895=CARTESIAN_POINT('Ctrl Pts',(80.8766815403268,-24.1788520286966,-8.88946106778054));
#11896=CARTESIAN_POINT('Ctrl Pts',(80.8579612709353,-21.8555160684168,-9.00059418577209));
#11897=CARTESIAN_POINT('Ctrl Pts',(82.7997191561016,-20.5796568486397,-9.11172730376366));
#11898=CARTESIAN_POINT('Ctrl Pts',(84.9247819526336,-21.5189909448313,-9.22286042175521));
#11899=CARTESIAN_POINT('Ctrl Pts',(85.2882085474095,-23.8138028202287,-9.33399353974677));
#11900=CARTESIAN_POINT('Ctrl Pts',(83.5573766165987,-25.3637903236025,-9.44512665773833));
#11901=CARTESIAN_POINT('Ctrl Pts',(81.3164116681401,-24.7503438849264,-9.55625977572988));
#11902=CARTESIAN_POINT('Ctrl Pts',(80.6163330263943,-22.5349138299059,-9.66739289372145));
#11903=CARTESIAN_POINT('Ctrl Pts',(82.0978802191083,-20.7451489433667,-9.77852601171301));
#11904=CARTESIAN_POINT('Ctrl Pts',(84.4050829423841,-21.0191124939321,-9.88965912970458));
#11905=CARTESIAN_POINT('Ctrl Pts',(85.4262984532635,-23.1060622570228,-10.0007922476961));
#11906=CARTESIAN_POINT('Ctrl Pts',(84.2268701215403,-25.0959396679168,-10.1119253656877));
#11907=CARTESIAN_POINT('Ctrl Pts',(81.9045619654454,-25.1675305993517,-10.2230584836792));
#11908=CARTESIAN_POINT('Ctrl Pts',(80.5848418145963,-23.255312213087,-10.3341916016708));
#11909=CARTESIAN_POINT('Ctrl Pts',(81.4755694947281,-21.1094220404143,-10.4453247196624));
#11910=CARTESIAN_POINT('Ctrl Pts',(83.7615159742851,-20.6938632287777,-10.5564578376539));
#11911=CARTESIAN_POINT('Ctrl Pts',(85.3504930611994,-22.3889715588227,-10.6675909556455));
#11912=CARTESIAN_POINT('Ctrl Pts',(84.7882063839989,-24.6433171680781,-10.778724073637));
#11913=CARTESIAN_POINT('Ctrl Pts',(82.5892828410451,-25.3936342247751,-10.8898571916286));
#11914=CARTESIAN_POINT('Ctrl Pts',(80.7662638076366,-23.9532030264328,-11.0009903096202));
#11915=CARTESIAN_POINT('Ctrl Pts',(80.987648056479,-21.6403629005937,-11.1121234276117));
#11916=CARTESIAN_POINT('Ctrl Pts',(83.0508160094325,-20.571916162926,-11.2232565456033));
#11917=CARTESIAN_POINT('Ctrl Pts',(85.0674751504547,-21.7257473213969,-11.3343896635948));
#11918=CARTESIAN_POINT('Ctrl Pts',(85.1918996587519,-24.0458246854221,-11.4455227815864));
#11919=CARTESIAN_POINT('Ctrl Pts',(83.3102113270295,-25.4087221340905,-11.556655899578));
#11920=CARTESIAN_POINT('Ctrl Pts',(81.1446053790108,-24.5670622792599,-11.6677890175695));
#11921=CARTESIAN_POINT('Ctrl Pts',(80.6771296157422,-22.2911653474804,-11.7789221355611));
#11922=CARTESIAN_POINT('Ctrl Pts',(82.3356362554336,-20.6640217891469,-11.8900552535526));
#11923=CARTESIAN_POINT('Ctrl Pts',(84.6021947432545,-21.1748574325926,-12.0011883715442));
#11924=CARTESIAN_POINT('Ctrl Pts',(85.4023615402782,-23.356135390641,-12.1123214895358));
#11925=CARTESIAN_POINT('Ctrl Pts',(84.0037924996106,-25.2114642218224,-12.2234546075273));
#11926=CARTESIAN_POINT('Ctrl Pts',(81.6865130544115,-25.0427739548083,-12.3345877255189));
#11927=CARTESIAN_POINT('Ctrl Pts',(80.5713885601575,-23.0044565615544,-12.4457208435104));
#11928=CARTESIAN_POINT('Ctrl Pts',(81.6790248448622,-20.9620603477572,-12.556853961502));
#11929=CARTESIAN_POINT('Ctrl Pts',(83.9956695846244,-20.7848667162158,-12.6679870794935));
#11930=CARTESIAN_POINT('Ctrl Pts',(85.4010383313655,-22.6350502527901,-12.7791201974851));
#11931=CARTESIAN_POINT('Ctrl Pts',(84.6088822932929,-24.819250162293,-12.8902533154767));
#11932=CARTESIAN_POINT('Ctrl Pts',(82.3442138554089,-25.3384007182767,-13.0013864334682));
#11933=CARTESIAN_POINT('Ctrl Pts',(80.6797467085456,-23.7173548983382,-13.1125195514598));
#11934=CARTESIAN_POINT('Ctrl Pts',(81.1388666983012,-21.4397576406269,-13.2236526694513));
#11935=CARTESIAN_POINT('Ctrl Pts',(83.301369139264,-20.5901556007548,-13.3347857874429));
#11936=CARTESIAN_POINT('Ctrl Pts',(85.1880466821996,-21.946138005623,-13.4459189054345));
#11937=CARTESIAN_POINT('Ctrl Pts',(85.0721377809063,-24.2666563873492,-13.557052023426));
#11938=CARTESIAN_POINT('Ctrl Pts',(83.0597268239821,-25.4278809882634,-13.6681851414176));
#11939=CARTESIAN_POINT('Ctrl Pts',(80.9926515269193,-24.3670133482552,-13.7793182594091));
#11940=CARTESIAN_POINT('Ctrl Pts',(80.7627805608964,-22.0550012868012,-13.8904513774007));
#11941=CARTESIAN_POINT('Ctrl Pts',(82.5805008816194,-20.6078892424568,-14.0015844953923));
#11942=CARTESIAN_POINT('Ctrl Pts',(84.7821633068503,-21.3501311159715,-14.1127176133838));
#11943=CARTESIAN_POINT('Ctrl Pts',(85.3527197283046,-23.6023979303683,-14.2238507313754));
#11944=CARTESIAN_POINT('Ctrl Pts',(83.769974452434,-25.3033264487149,-14.3349838493669));
#11945=CARTESIAN_POINT('Ctrl Pts',(81.4825182514663,-24.8961599432032,-14.4461169673585));
#11946=CARTESIAN_POINT('Ctrl Pts',(80.5839210749153,-22.7535532254418,-14.55725008535));
#11947=CARTESIAN_POINT('Ctrl Pts',(81.896614425227,-20.83650429601,-14.6683832033416));
#11948=CARTESIAN_POINT('Ctrl Pts',(84.2191696850261,-20.8995717888251,-14.7795163213332));
#11949=CARTESIAN_POINT('Ctrl Pts',(85.4258928578083,-22.8850338533659,-14.8906494393247));
#11950=CARTESIAN_POINT('Ctrl Pts',(84.4123434153425,-24.9757174587147,-15.0017825573163));
#11951=CARTESIAN_POINT('Ctrl Pts',(82.1061616690569,-25.2581466855875,-15.1129156753078));
#11952=CARTESIAN_POINT('Ctrl Pts',(80.6180559858753,-23.4738311795988,-15.2240487932994));
#11953=CARTESIAN_POINT('Ctrl Pts',(81.3099991340711,-21.2558467410411,-15.335181911291));
#11954=CARTESIAN_POINT('Ctrl Pts',(83.5486977575985,-20.6341799887301,-15.4463150292825));
#11955=CARTESIAN_POINT('Ctrl Pts',(85.2852062676543,-22.1778048794721,-15.5574481472741));
#11956=CARTESIAN_POINT('Ctrl Pts',(84.9302047132626,-24.4739350041461,-15.6685812652656));
#11957=CARTESIAN_POINT('Ctrl Pts',(82.8086025236948,-25.4210620022677,-15.7797143832572));
#11958=CARTESIAN_POINT('Ctrl Pts',(80.8621774495091,-24.1523373594438,-15.8908475012488));
#11959=CARTESIAN_POINT('Ctrl Pts',(80.8723665083473,-21.8289490162655,-16.0019806192403));
#11960=CARTESIAN_POINT('Ctrl Pts',(82.8298598709625,-20.5773510168392,-16.1131137372319));
#11961=CARTESIAN_POINT('Ctrl Pts',(84.9430514548956,-21.5430599298187,-16.2242468552234));
#11962=CARTESIAN_POINT('Ctrl Pts',(85.2779271980639,-23.842211340369,-16.335379973215));
#11963=CARTESIAN_POINT('Ctrl Pts',(83.5278718822138,-25.37055054633,-16.4465130912065));
#11964=CARTESIAN_POINT('Ctrl Pts',(81.2948518464886,-24.7292431320363,-16.5576462091981));
#11965=CARTESIAN_POINT('Ctrl Pts',(80.6221226098858,-22.5053151163976,-16.6687793271897));
#11966=CARTESIAN_POINT('Ctrl Pts',(82.1263744182192,-20.7340408632062,-16.7799124451812));
#11967=CARTESIAN_POINT('Ctrl Pts',(84.4288973912168,-21.0368642183003,-16.8910455631728));
#11968=CARTESIAN_POINT('Ctrl Pts',(85.4262515865763,-23.1360153040043,-17.0021786811644));
#11969=CARTESIAN_POINT('Ctrl Pts',(84.1976570595988,-25.1115842053849,-17.1133117991559));
#11970=CARTESIAN_POINT('Ctrl Pts',(82.656339145916,-25.1379171412778,-17.1874005444836));
#11971=CARTESIAN_POINT('Ctrl Pts',(82.0504464477385,-24.8221815534923,-17.2244449171475));
#11972=CARTESIAN_POINT('Ctrl Pts',(82.5032651029123,-24.8599788000028,-5.92518502761751));
#11973=CARTESIAN_POINT('Ctrl Pts',(81.8848044607624,-24.6948097220376,-5.96222940028136));
#11974=CARTESIAN_POINT('Ctrl Pts',(80.8363628652054,-23.7014089625658,-6.03631814560907));
#11975=CARTESIAN_POINT('Ctrl Pts',(81.2373204061652,-21.5588829416944,-6.14745126360063));
#11976=CARTESIAN_POINT('Ctrl Pts',(83.2546749765797,-20.7393325064207,-6.25858438159218));
#11977=CARTESIAN_POINT('Ctrl Pts',(85.0373946757938,-21.9868955223735,-6.36971749958375));
#11978=CARTESIAN_POINT('Ctrl Pts',(84.9561844212062,-24.1626575554218,-6.4808506175753));
#11979=CARTESIAN_POINT('Ctrl Pts',(83.084209310504,-25.2738257887494,-6.59198373556687));
#11980=CARTESIAN_POINT('Ctrl Pts',(81.1353569917424,-24.3041417188516,-6.70311685355843));
#11981=CARTESIAN_POINT('Ctrl Pts',(80.8930018437615,-22.1407342067759,-6.81424997154998));
#11982=CARTESIAN_POINT('Ctrl Pts',(82.5791032248387,-20.7638215423288,-6.92538308954155));
#11983=CARTESIAN_POINT('Ctrl Pts',(84.6504013903435,-21.4335168464905,-7.0365162075331));
#11984=CARTESIAN_POINT('Ctrl Pts',(85.211199533414,-23.5369345166976,-7.14764932552466));
#11985=CARTESIAN_POINT('Ctrl Pts',(83.7482146699515,-25.1489208985946,-7.25878244351622));
#11986=CARTESIAN_POINT('Ctrl Pts',(81.600437380424,-24.7941341465723,-7.36991556150778));
#11987=CARTESIAN_POINT('Ctrl Pts',(80.7335933376483,-22.7972832752565,-7.48104867949935));
#11988=CARTESIAN_POINT('Ctrl Pts',(81.9410546537625,-20.9859676979103,-7.59218179749089));
#11989=CARTESIAN_POINT('Ctrl Pts',(84.1177040410574,-21.0179732693197,-7.70331491548246));
#11990=CARTESIAN_POINT('Ctrl Pts',(85.271386892802,-22.8640079599594,-7.81444803347401));
#11991=CARTESIAN_POINT('Ctrl Pts',(84.3462069614533,-24.834507796152,-7.92558115146557));
#11992=CARTESIAN_POINT('Ctrl Pts',(82.1889254818703,-25.1259939529954,-8.03671426945713));
#11993=CARTESIAN_POINT('Ctrl Pts',(80.7739713002549,-23.47168673506,-8.14784738744869));
#11994=CARTESIAN_POINT('Ctrl Pts',(81.3963662126195,-21.3856732671765,-8.25898050544025));
#11995=CARTESIAN_POINT('Ctrl Pts',(83.4864698794196,-20.777155156739,-8.3701136234318));
#11996=CARTESIAN_POINT('Ctrl Pts',(85.1313371684087,-22.2030721410426,-8.48124674142337));
#11997=CARTESIAN_POINT('Ctrl Pts',(84.8255207907014,-24.3583688666995,-8.59237985941493));
#11998=CARTESIAN_POINT('Ctrl Pts',(82.8489159343259,-25.2704329416477,-8.70351297740649));
#11999=CARTESIAN_POINT('Ctrl Pts',(81.0105891610751,-24.1045074245427,-8.81464609539804));
#12000=CARTESIAN_POINT('Ctrl Pts',(80.9930494902522,-21.927693239752,-8.92577921338961));
#12001=CARTESIAN_POINT('Ctrl Pts',(82.8123499186543,-20.7322964074005,-9.03691233138116));
#12002=CARTESIAN_POINT('Ctrl Pts',(84.8033950873886,-21.6123911590012,-9.14804544937273));
#12003=CARTESIAN_POINT('Ctrl Pts',(85.1439020911812,-23.7624801376049,-9.25917856736428));
#12004=CARTESIAN_POINT('Ctrl Pts',(83.522225517973,-25.2147172833623,-9.37031168535584));
#12005=CARTESIAN_POINT('Ctrl Pts',(81.4225875961138,-24.6399580009559,-9.4814448033474));
#12006=CARTESIAN_POINT('Ctrl Pts',(80.7666595926412,-22.5642446079607,-9.59257792133896));
#12007=CARTESIAN_POINT('Ctrl Pts',(82.1547726334041,-20.887351700923,-9.70371103933052));
#12008=CARTESIAN_POINT('Ctrl Pts',(84.3164710279009,-21.1440376702283,-9.81484415732208));
#12009=CARTESIAN_POINT('Ctrl Pts',(85.2732833218679,-23.0993734137057,-9.92597727531363));
#12010=CARTESIAN_POINT('Ctrl Pts',(84.1494972441019,-24.9637586976604,-10.0371103933052));
#12011=CARTESIAN_POINT('Ctrl Pts',(81.9736460447631,-25.0308347287271,-10.1482435112968));
#12012=CARTESIAN_POINT('Ctrl Pts',(80.7371543821552,-23.2392108831868,-10.2593766292883));
#12013=CARTESIAN_POINT('Ctrl Pts',(81.5717080937345,-21.2286518221053,-10.3705097472799));
#12014=CARTESIAN_POINT('Ctrl Pts',(83.7134907749496,-20.8393003330179,-10.4816428652714));
#12015=CARTESIAN_POINT('Ctrl Pts',(85.2022586162076,-22.4275062234627,-10.592775983263));
#12016=CARTESIAN_POINT('Ctrl Pts',(84.675432691858,-24.5396809513299,-10.7039091012545));
#12017=CARTESIAN_POINT('Ctrl Pts',(82.6151848235318,-25.2426790712883,-10.8150422192461));
#12018=CARTESIAN_POINT('Ctrl Pts',(80.907134950887,-23.8930890342155,-10.9261753372377));
#12019=CARTESIAN_POINT('Ctrl Pts',(81.1145575455562,-21.7261087613869,-11.0373084552292));
#12020=CARTESIAN_POINT('Ctrl Pts',(83.0476112848241,-20.7250438900076,-11.1484415732208));
#12021=CARTESIAN_POINT('Ctrl Pts',(84.9370893022592,-21.8061083918933,-11.2595746912123));
#12022=CARTESIAN_POINT('Ctrl Pts',(85.0536669471746,-23.979869484634,-11.3707078092039));
#12023=CARTESIAN_POINT('Ctrl Pts',(83.2906477704926,-25.2568154577507,-11.4818409271955));
#12024=CARTESIAN_POINT('Ctrl Pts',(81.2616163144708,-24.468235096543,-11.592974045187));
#12025=CARTESIAN_POINT('Ctrl Pts',(80.8236220295607,-22.335868185809,-11.7041071631786));
#12026=CARTESIAN_POINT('Ctrl Pts',(82.3775345245986,-20.811340851396,-11.8152402811701));
#12027=CARTESIAN_POINT('Ctrl Pts',(84.5011519227265,-21.2899605145701,-11.9263733991617));
#12028=CARTESIAN_POINT('Ctrl Pts',(85.2508559964109,-23.3336756213079,-12.0375065171533));
#12029=CARTESIAN_POINT('Ctrl Pts',(83.9404880693515,-25.0719976660802,-12.1486396351448));
#12030=CARTESIAN_POINT('Ctrl Pts',(81.769348443972,-24.9139458938225,-12.2597727531364));
#12031=CARTESIAN_POINT('Ctrl Pts',(80.7245495606423,-23.0041755073622,-12.3709058711279));
#12032=CARTESIAN_POINT('Ctrl Pts',(81.7623324802696,-21.0905835322176,-12.4820389891195));
#12033=CARTESIAN_POINT('Ctrl Pts',(83.9328774280728,-20.9245646622873,-12.593172107111));
#12034=CARTESIAN_POINT('Ctrl Pts',(85.2496162360062,-22.6580659017705,-12.7043052251026));
#12035=CARTESIAN_POINT('Ctrl Pts',(84.5074177207144,-24.7045186863484,-12.8154383430942));
#12036=CARTESIAN_POINT('Ctrl Pts',(82.3855711760416,-25.1909288799784,-12.9265714610857));
#12037=CARTESIAN_POINT('Ctrl Pts',(80.8260740747382,-23.6721147285318,-13.0377045790773));
#12038=CARTESIAN_POINT('Ctrl Pts',(81.2562395451253,-21.5381547233549,-13.1488376970688));
#12039=CARTESIAN_POINT('Ctrl Pts',(83.282363217556,-20.7421330530331,-13.2599708150604));
#12040=CARTESIAN_POINT('Ctrl Pts',(85.0500569595722,-22.0126000813523,-13.371103933052));
#12041=CARTESIAN_POINT('Ctrl Pts',(84.941457882731,-24.1867743789001,-13.4822370510435));
#12042=CARTESIAN_POINT('Ctrl Pts',(83.0559601365792,-25.2747660538938,-13.5933701690351));
#12043=CARTESIAN_POINT('Ctrl Pts',(81.1192454708557,-24.2808023024453,-13.7045032870266));
#12044=CARTESIAN_POINT('Ctrl Pts',(80.9038713759918,-22.1145978719098,-13.8156364050182));
#12045=CARTESIAN_POINT('Ctrl Pts',(82.6069567006193,-20.7587483180938,-13.9267695230098));
#12046=CARTESIAN_POINT('Ctrl Pts',(84.6697707229126,-21.4541805183588,-14.0379026410013));
#12047=CARTESIAN_POINT('Ctrl Pts',(85.2043448579832,-23.5644075510958,-14.1490357589929));
#12048=CARTESIAN_POINT('Ctrl Pts',(83.7214158170148,-25.1580665781811,-14.2601688769844));
#12049=CARTESIAN_POINT('Ctrl Pts',(81.5782186253548,-24.7765781322903,-14.371301994976));
#12050=CARTESIAN_POINT('Ctrl Pts',(80.7362917091574,-22.7690954541978,-14.4824351129676));
#12051=CARTESIAN_POINT('Ctrl Pts',(81.9661997181974,-20.9729457049286,-14.5935682309591));
#12052=CARTESIAN_POINT('Ctrl Pts',(84.1422824375826,-21.0320358302079,-14.7047013489507));
#12053=CARTESIAN_POINT('Ctrl Pts',(85.2729033053935,-22.8922842227546,-14.8158344669423));
#12054=CARTESIAN_POINT('Ctrl Pts',(84.3232736172787,-24.8511183327747,-14.9269675849338));
#12055=CARTESIAN_POINT('Ctrl Pts',(82.1625318115973,-25.1157360883498,-15.0381007029254));
#12056=CARTESIAN_POINT('Ctrl Pts',(80.768273893243,-23.443948895287,-15.1492338209169));
#12057=CARTESIAN_POINT('Ctrl Pts',(81.4165794701427,-21.3658422116044,-15.2603669389085));
#12058=CARTESIAN_POINT('Ctrl Pts',(83.5140939934316,-20.7833810317412,-15.3715000569));
#12059=CARTESIAN_POINT('Ctrl Pts',(85.1410891509651,-22.2296568246568,-15.4826331748916));
#12060=CARTESIAN_POINT('Ctrl Pts',(84.8084758602341,-24.38098091681,-15.5937662928831));
#12061=CARTESIAN_POINT('Ctrl Pts',(82.8206730544022,-25.2683771089908,-15.7048994108747));
#12062=CARTESIAN_POINT('Ctrl Pts',(80.9969997744478,-24.0796649096756,-15.8160325288663));
#12063=CARTESIAN_POINT('Ctrl Pts',(81.0065462576891,-21.9028016455272,-15.9271656468578));
#12064=CARTESIAN_POINT('Ctrl Pts',(82.8405898016374,-20.7301359934712,-16.0382987648494));
#12065=CARTESIAN_POINT('Ctrl Pts',(84.8205124188263,-21.6349422273054,-16.1494318828409));
#12066=CARTESIAN_POINT('Ctrl Pts',(85.1342691377567,-23.7890970671697,-16.2605650008325));
#12067=CARTESIAN_POINT('Ctrl Pts',(83.494581507195,-25.2210511709176,-16.371698118824));
#12068=CARTESIAN_POINT('Ctrl Pts',(81.4023874501187,-24.6201879724339,-16.4828312368156));
#12069=CARTESIAN_POINT('Ctrl Pts',(80.7720840545721,-22.5365125448765,-16.5939643548072));
#12070=CARTESIAN_POINT('Ctrl Pts',(82.1814698385731,-20.8769441546737,-16.7050974727988));
#12071=CARTESIAN_POINT('Ctrl Pts',(84.3387836124383,-21.1606698775672,-16.8162305907903));
#12072=CARTESIAN_POINT('Ctrl Pts',(85.27323941084,-23.1274374641322,-16.9273637087819));
#12073=CARTESIAN_POINT('Ctrl Pts',(84.1221265113701,-24.9784166083791,-17.0384968267734));
#12074=CARTESIAN_POINT('Ctrl Pts',(82.6780122054164,-25.003088850947,-17.1125855721011));
#12075=CARTESIAN_POINT('Ctrl Pts',(82.1103302849355,-24.7072652086133,-17.149629944765));
#12076=CARTESIAN_POINT('Ctrl Pts',(82.5367004230132,-24.7347832743338,-5.85037005523502));
#12077=CARTESIAN_POINT('Ctrl Pts',(81.9598684839428,-24.5807317583216,-5.88741442789887));
#12078=CARTESIAN_POINT('Ctrl Pts',(80.9819976909611,-23.6541969923126,-5.96150317322658));
#12079=CARTESIAN_POINT('Ctrl Pts',(81.3559667038196,-21.6558848041161,-6.07263629121814));
#12080=CARTESIAN_POINT('Ctrl Pts',(83.2375327556212,-20.8914984640225,-6.1837694092097));
#12081=CARTESIAN_POINT('Ctrl Pts',(84.9002572538884,-22.0550877768411,-6.29490252720125));
#12082=CARTESIAN_POINT('Ctrl Pts',(84.8245132769339,-24.0843988549335,-6.40603564519282));
#12083=CARTESIAN_POINT('Ctrl Pts',(83.0785411658485,-25.120774143805,-6.51716876318437));
#12084=CARTESIAN_POINT('Ctrl Pts',(81.2608664661531,-24.2163596924983,-6.62830188117594));
#12085=CARTESIAN_POINT('Ctrl Pts',(81.0348242891322,-22.1985715502295,-6.73943499916749));
#12086=CARTESIAN_POINT('Ctrl Pts',(82.6074338665743,-20.9143391382806,-6.85056811715906));
#12087=CARTESIAN_POINT('Ctrl Pts',(84.5393125598535,-21.5389571245491,-6.9617012351506));
#12088=CARTESIAN_POINT('Ctrl Pts',(85.0623632735896,-23.5007933525791,-7.07283435314218));
#12089=CARTESIAN_POINT('Ctrl Pts',(83.6978521986601,-25.0042766254877,-7.18396747113372));
#12090=CARTESIAN_POINT('Ctrl Pts',(81.6946422056962,-24.6733706370095,-7.29510058912529));
#12091=CARTESIAN_POINT('Ctrl Pts',(80.8861455997883,-22.8109281764329,-7.40623370711685));
#12092=CARTESIAN_POINT('Ctrl Pts',(82.0123324657874,-21.1215325940124,-7.5173668251084));
#12093=CARTESIAN_POINT('Ctrl Pts',(84.0424711701439,-21.1513838643421,-7.62849994309997));
#12094=CARTESIAN_POINT('Ctrl Pts',(85.1184994104062,-22.8731616099578,-7.73963306109152));
#12095=CARTESIAN_POINT('Ctrl Pts',(84.2555935156453,-24.7110267285814,-7.85076617908309));
#12096=CARTESIAN_POINT('Ctrl Pts',(82.2435190614604,-24.9828928969436,-7.96189929707464));
#12097=CARTESIAN_POINT('Ctrl Pts',(80.9238057140765,-23.4399374114941,-8.0730324150662));
#12098=CARTESIAN_POINT('Ctrl Pts',(81.5043071068873,-21.4943339056295,-8.18416553305776));
#12099=CARTESIAN_POINT('Ctrl Pts',(83.4537254996042,-20.9267752645769,-8.29529865104932));
#12100=CARTESIAN_POINT('Ctrl Pts',(84.9878764595144,-22.2567135063218,-8.40643176904088));
#12101=CARTESIAN_POINT('Ctrl Pts',(84.7026446401716,-24.2669368007434,-8.51756488703244));
#12102=CARTESIAN_POINT('Ctrl Pts',(82.859085431431,-25.117609669885,-8.628698005024));
#12103=CARTESIAN_POINT('Ctrl Pts',(81.1444967818236,-24.0301628203888,-8.73983112301555));
#12104=CARTESIAN_POINT('Ctrl Pts',(81.1281377095688,-21.9998704110872,-8.85096424100712));
#12105=CARTESIAN_POINT('Ctrl Pts',(82.8249806812072,-20.8849359661613,-8.96209735899867));
#12106=CARTESIAN_POINT('Ctrl Pts',(84.6820082221436,-21.7057913731711,-9.07323047699025));
#12107=CARTESIAN_POINT('Ctrl Pts',(84.9995956349529,-23.7111574549811,-9.18436359498178));
#12108=CARTESIAN_POINT('Ctrl Pts',(83.4870744193475,-25.0656442431221,-9.29549671297336));
#12109=CARTESIAN_POINT('Ctrl Pts',(81.5287635240873,-24.5295721169854,-9.40662983096491));
#12110=CARTESIAN_POINT('Ctrl Pts',(80.9169861588886,-22.5935753860154,-9.51776294895647));
#12111=CARTESIAN_POINT('Ctrl Pts',(82.2116650476995,-21.0295544584792,-9.62889606694803));
#12112=CARTESIAN_POINT('Ctrl Pts',(84.227859113418,-21.2689628465245,-9.74002918493959));
#12113=CARTESIAN_POINT('Ctrl Pts',(85.1202681904721,-23.0926845703885,-9.85116230293114));
#12114=CARTESIAN_POINT('Ctrl Pts',(84.0721243666637,-24.8315777274041,-9.96229542092271));
#12115=CARTESIAN_POINT('Ctrl Pts',(82.0427301240806,-24.8941388581025,-10.0734285389143));
#12116=CARTESIAN_POINT('Ctrl Pts',(80.8894669497142,-23.2231095532865,-10.1845616569058));
#12117=CARTESIAN_POINT('Ctrl Pts',(81.6678466927408,-21.3478816037963,-10.2956947748974));
#12118=CARTESIAN_POINT('Ctrl Pts',(83.6654655756142,-20.9847374372581,-10.4068278928889));
#12119=CARTESIAN_POINT('Ctrl Pts',(85.0540241712157,-22.4660408881028,-10.5179610108805));
#12120=CARTESIAN_POINT('Ctrl Pts',(84.5626589997171,-24.4360447345817,-10.629094128872));
#12121=CARTESIAN_POINT('Ctrl Pts',(82.6410868060184,-25.0917239178013,-10.7402272468636));
#12122=CARTESIAN_POINT('Ctrl Pts',(81.0480060941376,-23.8329750419982,-10.8513603648552));
#12123=CARTESIAN_POINT('Ctrl Pts',(81.2414670346331,-21.81185462218,-10.9624934828467));
#12124=CARTESIAN_POINT('Ctrl Pts',(83.0444065602159,-20.8781716170892,-11.0736266008383));
#12125=CARTESIAN_POINT('Ctrl Pts',(84.8067034540636,-21.8864694623896,-11.1847597188299));
#12126=CARTESIAN_POINT('Ctrl Pts',(84.9154342355974,-23.913914283846,-11.2958928368214));
#12127=CARTESIAN_POINT('Ctrl Pts',(83.2710842139556,-25.1049087814108,-11.407025954813));
#12128=CARTESIAN_POINT('Ctrl Pts',(81.3786272499309,-24.3694079138262,-11.5181590728045));
#12129=CARTESIAN_POINT('Ctrl Pts',(80.9701144433791,-22.3805710241376,-11.6292921907961));
#12130=CARTESIAN_POINT('Ctrl Pts',(82.4194327937636,-20.9586599136451,-11.7404253087876));
#12131=CARTESIAN_POINT('Ctrl Pts',(84.4001091021983,-21.4050635965476,-11.8515584267792));
#12132=CARTESIAN_POINT('Ctrl Pts',(85.0993504525439,-23.3112158519747,-11.9626915447708));
#12133=CARTESIAN_POINT('Ctrl Pts',(83.8771836390926,-24.9325311103381,-12.0738246627623));
#12134=CARTESIAN_POINT('Ctrl Pts',(81.8521838335323,-24.7851178328367,-12.1849577807539));
#12135=CARTESIAN_POINT('Ctrl Pts',(80.8777105611273,-23.00389445317,-12.2960908987455));
#12136=CARTESIAN_POINT('Ctrl Pts',(81.8456401156769,-21.2191067166779,-12.407224016737));
#12137=CARTESIAN_POINT('Ctrl Pts',(83.8700852715213,-21.0642626083588,-12.5183571347286));
#12138=CARTESIAN_POINT('Ctrl Pts',(85.0981941406469,-22.681081550751,-12.6294902527201));
#12139=CARTESIAN_POINT('Ctrl Pts',(84.4059531481358,-24.5897872104038,-12.7406233707117));
#12140=CARTESIAN_POINT('Ctrl Pts',(82.4269284966742,-25.0434570416802,-12.8517564887032));
#12141=CARTESIAN_POINT('Ctrl Pts',(80.9724014409309,-23.6268745587255,-12.9628896066948));
#12142=CARTESIAN_POINT('Ctrl Pts',(81.3736123919494,-21.636551806083,-13.0740227246864));
#12143=CARTESIAN_POINT('Ctrl Pts',(83.263357295848,-20.8941105053114,-13.1851558426779));
#12144=CARTESIAN_POINT('Ctrl Pts',(84.912067236945,-22.0790621570815,-13.2962889606695));
#12145=CARTESIAN_POINT('Ctrl Pts',(84.8107779845556,-24.1068923704511,-13.407422078661));
#12146=CARTESIAN_POINT('Ctrl Pts',(83.0521934491764,-25.1216511195243,-13.5185551966526));
#12147=CARTESIAN_POINT('Ctrl Pts',(81.2458394147922,-24.1945912566353,-13.6296883146442));
#12148=CARTESIAN_POINT('Ctrl Pts',(81.0449621910871,-22.1741944570185,-13.7408214326357));
#12149=CARTESIAN_POINT('Ctrl Pts',(82.6334125196193,-20.9096073937307,-13.8519545506273));
#12150=CARTESIAN_POINT('Ctrl Pts',(84.5573781389748,-21.5582299207461,-13.9630876686188));
#12151=CARTESIAN_POINT('Ctrl Pts',(85.055969987662,-23.5264171718233,-14.0742207866104));
#12152=CARTESIAN_POINT('Ctrl Pts',(83.6728571815953,-25.0128067076473,-14.1853539046019));
#12153=CARTESIAN_POINT('Ctrl Pts',(81.6739189992434,-24.6569963213773,-14.2964870225935));
#12154=CARTESIAN_POINT('Ctrl Pts',(80.8886623433994,-22.7846376829539,-14.4076201405851));
#12155=CARTESIAN_POINT('Ctrl Pts',(82.0357850111679,-21.1093871138471,-14.5187532585766));
#12156=CARTESIAN_POINT('Ctrl Pts',(84.0653951901389,-21.1644998715908,-14.6298863765682));
#12157=CARTESIAN_POINT('Ctrl Pts',(85.1199137529788,-22.8995345921432,-14.7410194945598));
#12158=CARTESIAN_POINT('Ctrl Pts',(84.234203819215,-24.7265192068348,-14.8521526125513));
#12159=CARTESIAN_POINT('Ctrl Pts',(82.2189019541376,-24.9733254911122,-14.9632857305429));
#12160=CARTESIAN_POINT('Ctrl Pts',(80.9184918006105,-23.4140666109752,-15.0744188485344));
#12161=CARTESIAN_POINT('Ctrl Pts',(81.5231598062145,-21.4758376821678,-15.185551966526));
#12162=CARTESIAN_POINT('Ctrl Pts',(83.4794902292645,-20.9325820747523,-15.2966850845175));
#12163=CARTESIAN_POINT('Ctrl Pts',(84.9969720342762,-22.2815087698416,-15.4078182025091));
#12164=CARTESIAN_POINT('Ctrl Pts',(84.6867470072055,-24.2880268294738,-15.5189513205007));
#12165=CARTESIAN_POINT('Ctrl Pts',(82.8327435851099,-25.1156922157141,-15.6300844384922));
#12166=CARTESIAN_POINT('Ctrl Pts',(81.1318220993863,-24.0069924599074,-15.7412175564838));
#12167=CARTESIAN_POINT('Ctrl Pts',(81.140726007031,-21.976654274789,-15.8523506744753));
#12168=CARTESIAN_POINT('Ctrl Pts',(82.8513197323124,-20.8829209701032,-15.9634837924669));
#12169=CARTESIAN_POINT('Ctrl Pts',(84.6979733827568,-21.7268245247922,-16.0746169104585));
#12170=CARTESIAN_POINT('Ctrl Pts',(84.9906110774499,-23.7359827939705,-16.18575002845));
#12171=CARTESIAN_POINT('Ctrl Pts',(83.4612911321759,-25.0715517955052,-16.2968831464416));
#12172=CARTESIAN_POINT('Ctrl Pts',(81.5099230537491,-24.5111328128315,-16.4080162644331));
#12173=CARTESIAN_POINT('Ctrl Pts',(80.9220454992582,-22.5677099733552,-16.5191493824247));
#12174=CARTESIAN_POINT('Ctrl Pts',(82.2365652589273,-21.0198474461412,-16.6302825004163));
#12175=CARTESIAN_POINT('Ctrl Pts',(84.2486698336597,-21.2844755368341,-16.7414156184078));
#12176=CARTESIAN_POINT('Ctrl Pts',(85.120227235104,-23.1188596242601,-16.8525487363994));
#12177=CARTESIAN_POINT('Ctrl Pts',(84.0465959631413,-24.8452490113732,-16.9636818543909));
#12178=CARTESIAN_POINT('Ctrl Pts',(82.6996852649168,-24.8682605606161,-17.0377705997186));
#12179=CARTESIAN_POINT('Ctrl Pts',(82.1702141221325,-24.5923488637344,-17.0748149723825));
#12180=CARTESIAN_POINT('Ctrl Pts',(82.5701357431142,-24.6095877486648,-5.77555508285253));
#12181=CARTESIAN_POINT('Ctrl Pts',(82.0349325071233,-24.4666537946055,-5.81259945551638));
#12182=CARTESIAN_POINT('Ctrl Pts',(81.1276325167165,-23.6069850220594,-5.88668820084409));
#12183=CARTESIAN_POINT('Ctrl Pts',(81.4746130014742,-21.7528866665377,-5.99782131883565));
#12184=CARTESIAN_POINT('Ctrl Pts',(83.2203905346628,-21.0436644216242,-6.10895443682721));
#12185=CARTESIAN_POINT('Ctrl Pts',(84.7631198319829,-22.1232800313086,-6.22008755481877));
#12186=CARTESIAN_POINT('Ctrl Pts',(84.6928421326618,-24.0061401544452,-6.33122067281032));
#12187=CARTESIAN_POINT('Ctrl Pts',(83.0728730211929,-24.9677224988606,-6.44235379080189));
#12188=CARTESIAN_POINT('Ctrl Pts',(81.3863759405641,-24.1285776661449,-6.55348690879345));
#12189=CARTESIAN_POINT('Ctrl Pts',(81.1766467345028,-22.256408893683,-6.66462002678501));
#12190=CARTESIAN_POINT('Ctrl Pts',(82.6357645083098,-21.0648567342324,-6.77575314477657));
#12191=CARTESIAN_POINT('Ctrl Pts',(84.4282237293633,-21.6443974026076,-6.88688626276812));
#12192=CARTESIAN_POINT('Ctrl Pts',(84.9135270137654,-23.4646521884607,-6.99801938075969));
#12193=CARTESIAN_POINT('Ctrl Pts',(83.6474897273688,-24.8596323523809,-7.10915249875124));
#12194=CARTESIAN_POINT('Ctrl Pts',(81.7888470309685,-24.5526071274467,-7.2202856167428));
#12195=CARTESIAN_POINT('Ctrl Pts',(81.0386978619283,-22.8245730776092,-7.33141873473436));
#12196=CARTESIAN_POINT('Ctrl Pts',(82.0836102778123,-21.2570974901144,-7.44255185272592));
#12197=CARTESIAN_POINT('Ctrl Pts',(83.9672382992303,-21.2847944593645,-7.55368497071748));
#12198=CARTESIAN_POINT('Ctrl Pts',(84.9656119280105,-22.8823152599562,-7.66481808870903));
#12199=CARTESIAN_POINT('Ctrl Pts',(84.164980069837,-24.5875456610108,-7.7759512067006));
#12200=CARTESIAN_POINT('Ctrl Pts',(82.2981126410506,-24.8397918408919,-7.88708432469216));
#12201=CARTESIAN_POINT('Ctrl Pts',(81.0736401278978,-23.4081880879282,-7.99821744268371));
#12202=CARTESIAN_POINT('Ctrl Pts',(81.6122480011553,-21.6029945440825,-8.10935056067529));
#12203=CARTESIAN_POINT('Ctrl Pts',(83.4209811197886,-21.0763953724148,-8.22048367866682));
#12204=CARTESIAN_POINT('Ctrl Pts',(84.8444157506201,-22.3103548716009,-8.3316167966584));
#12205=CARTESIAN_POINT('Ctrl Pts',(84.5797684896418,-24.1755047347873,-8.44274991464994));
#12206=CARTESIAN_POINT('Ctrl Pts',(82.8692549285362,-24.9647863981223,-8.55388303264151));
#12207=CARTESIAN_POINT('Ctrl Pts',(81.2784044025718,-23.9558182162349,-8.66501615063306));
#12208=CARTESIAN_POINT('Ctrl Pts',(81.2632259288858,-22.0720475824224,-8.77614926862463));
#12209=CARTESIAN_POINT('Ctrl Pts',(82.8376114437597,-21.0375755249222,-8.88728238661619));
#12210=CARTESIAN_POINT('Ctrl Pts',(84.5606213568987,-21.799191587341,-8.99841550460775));
#12211=CARTESIAN_POINT('Ctrl Pts',(84.8552891787246,-23.6598347723572,-9.10954862259931));
#12212=CARTESIAN_POINT('Ctrl Pts',(83.4519233207219,-24.9165712028819,-9.22068174059086));
#12213=CARTESIAN_POINT('Ctrl Pts',(81.6349394520607,-24.419186233015,-9.33181485858243));
#12214=CARTESIAN_POINT('Ctrl Pts',(81.0673127251357,-22.6229061640702,-9.44294797657398));
#12215=CARTESIAN_POINT('Ctrl Pts',(82.2685574619953,-21.1717572160355,-9.55408109456555));
#12216=CARTESIAN_POINT('Ctrl Pts',(84.139247198935,-21.3938880228207,-9.66521421255709));
#12217=CARTESIAN_POINT('Ctrl Pts',(84.9672530590764,-23.0859957270714,-9.77634733054866));
#12218=CARTESIAN_POINT('Ctrl Pts',(83.9947514892254,-24.6993967571477,-9.88748044854022));
#12219=CARTESIAN_POINT('Ctrl Pts',(82.1118142033981,-24.7574429874778,-9.99861356653178));
#12220=CARTESIAN_POINT('Ctrl Pts',(81.0417795172734,-23.2070082233863,-10.1097466845233));
#12221=CARTESIAN_POINT('Ctrl Pts',(81.7639852917469,-21.4671113854874,-10.2208798025149));
#12222=CARTESIAN_POINT('Ctrl Pts',(83.6174403762788,-21.1301745414983,-10.3320129205065));
#12223=CARTESIAN_POINT('Ctrl Pts',(84.9057897262238,-22.5045755527429,-10.443146038498));
#12224=CARTESIAN_POINT('Ctrl Pts',(84.4498853075762,-24.3324085178334,-10.5542791564896));
#12225=CARTESIAN_POINT('Ctrl Pts',(82.6669887885052,-24.9407687643145,-10.6654122744811));
#12226=CARTESIAN_POINT('Ctrl Pts',(81.1888772373878,-23.7728610497808,-10.7765453924727));
#12227=CARTESIAN_POINT('Ctrl Pts',(81.3683765237105,-21.8976004829732,-10.8876785104643));
#12228=CARTESIAN_POINT('Ctrl Pts',(83.0412018356075,-21.0312993441707,-10.9988116284558));
#12229=CARTESIAN_POINT('Ctrl Pts',(84.6763176058681,-21.9668305328859,-11.1099447464474));
#12230=CARTESIAN_POINT('Ctrl Pts',(84.7772015240203,-23.8479590830579,-11.2210778644389));
#12231=CARTESIAN_POINT('Ctrl Pts',(83.2515206574186,-24.953002105071,-11.3322109824305));
#12232=CARTESIAN_POINT('Ctrl Pts',(81.495638185391,-24.2705807311094,-11.443344100422));
#12233=CARTESIAN_POINT('Ctrl Pts',(81.1166068571975,-22.4252738624662,-11.5544772184136));
#12234=CARTESIAN_POINT('Ctrl Pts',(82.4613310629286,-21.1059789758943,-11.6656103364052));
#12235=CARTESIAN_POINT('Ctrl Pts',(84.2990662816703,-21.520166678525,-11.7767434543967));
#12236=CARTESIAN_POINT('Ctrl Pts',(84.9478449086767,-23.2887560826416,-11.8878765723883));
#12237=CARTESIAN_POINT('Ctrl Pts',(83.8138792088337,-24.793064554596,-11.9990096903798));
#12238=CARTESIAN_POINT('Ctrl Pts',(81.9350192230927,-24.6562897718509,-12.1101428083714));
#12239=CARTESIAN_POINT('Ctrl Pts',(81.0308715616122,-23.0036133989778,-12.221275926363));
#12240=CARTESIAN_POINT('Ctrl Pts',(81.9289477510842,-21.3476299011382,-12.3324090443545));
#12241=CARTESIAN_POINT('Ctrl Pts',(83.8072931149699,-21.2039605544302,-12.4435421623461));
#12242=CARTESIAN_POINT('Ctrl Pts',(84.9467720452876,-22.7040971997315,-12.5546752803376));
#12243=CARTESIAN_POINT('Ctrl Pts',(84.3044885755572,-24.4750557344592,-12.6658083983292));
#12244=CARTESIAN_POINT('Ctrl Pts',(82.4682858173069,-24.8959852033819,-12.7769415163208));
#12245=CARTESIAN_POINT('Ctrl Pts',(81.1187288071235,-23.5816343889191,-12.8880746343123));
#12246=CARTESIAN_POINT('Ctrl Pts',(81.4909852387734,-21.734948888811,-12.9992077523039));
#12247=CARTESIAN_POINT('Ctrl Pts',(83.24435137414,-21.0460879575897,-13.1103408702954));
#12248=CARTESIAN_POINT('Ctrl Pts',(84.7740775143177,-22.1455242328108,-13.221473988287));
#12249=CARTESIAN_POINT('Ctrl Pts',(84.6800980863804,-24.027010362002,-13.3326071062785));
#12250=CARTESIAN_POINT('Ctrl Pts',(83.0484267617735,-24.9685361851548,-13.4437402242701));
#12251=CARTESIAN_POINT('Ctrl Pts',(81.3724333587286,-24.1083802108253,-13.5548733422617));
#12252=CARTESIAN_POINT('Ctrl Pts',(81.1860530061824,-22.2337910421272,-13.6660064602532));
#12253=CARTESIAN_POINT('Ctrl Pts',(82.6598683386192,-21.0604664693676,-13.7771395782448));
#12254=CARTESIAN_POINT('Ctrl Pts',(84.4449855550371,-21.6622793231335,-13.8882726962364));
#12255=CARTESIAN_POINT('Ctrl Pts',(84.9075951173406,-23.4884267925507,-13.9994058142279));
#12256=CARTESIAN_POINT('Ctrl Pts',(83.6242985461759,-24.8675468371136,-14.1105389322195));
#12257=CARTESIAN_POINT('Ctrl Pts',(81.769619373132,-24.5374145104643,-14.221672050211));
#12258=CARTESIAN_POINT('Ctrl Pts',(81.0410329776415,-22.80017991171,-14.3328051682026));
#12259=CARTESIAN_POINT('Ctrl Pts',(82.1053703041383,-21.2458285227657,-14.4439382861941));
#12260=CARTESIAN_POINT('Ctrl Pts',(83.9885079426954,-21.2969639129736,-14.5550714041857));
#12261=CARTESIAN_POINT('Ctrl Pts',(84.9669242005639,-22.9067849615319,-14.6662045221773));
#12262=CARTESIAN_POINT('Ctrl Pts',(84.1451340211513,-24.6019200808948,-14.7773376401688));
#12263=CARTESIAN_POINT('Ctrl Pts',(82.275272096678,-24.8309148938745,-14.8884707581604));
#12264=CARTESIAN_POINT('Ctrl Pts',(81.0687097079781,-23.3841843266634,-14.9996038761519));
#12265=CARTESIAN_POINT('Ctrl Pts',(81.6297401422862,-21.5858331527312,-15.1107369941435));
#12266=CARTESIAN_POINT('Ctrl Pts',(83.4448864650975,-21.0817831177634,-15.221870112135));
#12267=CARTESIAN_POINT('Ctrl Pts',(84.8528549175871,-22.3333607150264,-15.3330032301266));
#12268=CARTESIAN_POINT('Ctrl Pts',(84.565018154177,-24.1950727421377,-15.4441363481182));
#12269=CARTESIAN_POINT('Ctrl Pts',(82.8448141158174,-24.9630073224372,-15.5552694661097));
#12270=CARTESIAN_POINT('Ctrl Pts',(81.2666444243251,-23.9343200101391,-15.6664025841013));
#12271=CARTESIAN_POINT('Ctrl Pts',(81.2749057563727,-22.0505069040507,-15.7775357020928));
#12272=CARTESIAN_POINT('Ctrl Pts',(82.8620496629874,-21.0357059467352,-15.8886688200844));
#12273=CARTESIAN_POINT('Ctrl Pts',(84.5754343466875,-21.818706822279,-15.999801938076));
#12274=CARTESIAN_POINT('Ctrl Pts',(84.8469530171428,-23.6828685207713,-16.1109350560675));
#12275=CARTESIAN_POINT('Ctrl Pts',(83.428000757157,-24.9220524200928,-16.2220681740591));
#12276=CARTESIAN_POINT('Ctrl Pts',(81.6174586573793,-24.4020776532291,-16.3332012920507));
#12277=CARTESIAN_POINT('Ctrl Pts',(81.0720069439444,-22.598907401834,-16.4443344100422));
#12278=CARTESIAN_POINT('Ctrl Pts',(82.2916606792813,-21.1627507376087,-16.5554675280338));
#12279=CARTESIAN_POINT('Ctrl Pts',(84.1585560548812,-21.4082811961009,-16.6666006460253));
#12280=CARTESIAN_POINT('Ctrl Pts',(84.9672150593679,-23.1102817843879,-16.7777337640169));
#12281=CARTESIAN_POINT('Ctrl Pts',(83.9710654149125,-24.7120814143673,-16.8888668820084));
#12282=CARTESIAN_POINT('Ctrl Pts',(82.7213583244171,-24.7334322702853,-16.9629556273361));
#12283=CARTESIAN_POINT('Ctrl Pts',(82.2300979593295,-24.4774325188554,-17.));
#12284=CARTESIAN_POINT('Ctrl Pts',(81.3361555725406,-22.9990558295284,-6.62148036339021));
#12285=CARTESIAN_POINT('Ctrl Pts',(81.3350366720467,-22.7833631289824,-6.63586025118848));
#12286=CARTESIAN_POINT('Ctrl Pts',(81.3739566040229,-22.5680575720948,-6.65024013898675));
#12287=CARTESIAN_POINT('Ctrl Pts',(81.4547878978142,-22.3698449958516,-6.66462002678502));
#12288=CARTESIAN_POINT('Ctrl Pts',(81.6630193257718,-21.8592248405328,-6.70166439944887));
#12289=CARTESIAN_POINT('Ctrl Pts',(82.1493919170408,-21.4620407873826,-6.73870877211272));
#12290=CARTESIAN_POINT('Ctrl Pts',(82.6913214161842,-21.3600388722033,-6.77575314477657));
#12291=CARTESIAN_POINT('Ctrl Pts',(83.2332509153276,-21.2580369570241,-6.81279751744043));
#12292=CARTESIAN_POINT('Ctrl Pts',(83.8307373223455,-21.4512171798158,-6.84984189010428));
#12293=CARTESIAN_POINT('Ctrl Pts',(84.2103644065881,-21.8511830888539,-6.88688626276813));
#12294=CARTESIAN_POINT('Ctrl Pts',(84.5899914908307,-22.2511489978919,-6.92393063543198));
#12295=CARTESIAN_POINT('Ctrl Pts',(84.751759252298,-22.8579005931763,-6.96097500809584));
#12296=CARTESIAN_POINT('Ctrl Pts',(84.6216369186323,-23.3937730848052,-6.99801938075969));
#12297=CARTESIAN_POINT('Ctrl Pts',(84.4915145849665,-23.9296455764341,-7.03506375342355));
#12298=CARTESIAN_POINT('Ctrl Pts',(84.0695021561676,-24.3946389644075,-7.0721081260874));
#12299=CARTESIAN_POINT('Ctrl Pts',(83.5487221590348,-24.5759647875718,-7.10915249875125));
#12300=CARTESIAN_POINT('Ctrl Pts',(83.027942161902,-24.7572906107362,-7.1461968714151));
#12301=CARTESIAN_POINT('Ctrl Pts',(82.4083945964353,-24.6549488690914,-7.18324124407896));
#12302=CARTESIAN_POINT('Ctrl Pts',(81.9735959521952,-24.3157723232961,-7.22028561674281));
#12303=CARTESIAN_POINT('Ctrl Pts',(81.5776803201884,-24.0069275321053,-7.25401719895861));
#12304=CARTESIAN_POINT('Ctrl Pts',(81.3349477858388,-23.5017130479715,-7.28774878117441));
#12305=CARTESIAN_POINT('Ctrl Pts',(81.3317907907837,-22.9991411291167,-7.32148036339021));
#12306=CARTESIAN_POINT('Ctrl Pts',(82.4698297828114,-24.9851743256717,-6.));
#12307=CARTESIAN_POINT('Ctrl Pts',(82.4011651403016,-24.9597503542562,-6.));
#12308=CARTESIAN_POINT('Ctrl Pts',(82.3342038415895,-24.9304366816692,-6.));
#12309=CARTESIAN_POINT('Ctrl Pts',(82.2691348210017,-24.897527340086,-6.));
#12310=CARTESIAN_POINT('Ctrl Pts',(82.2022547374464,-24.8637020343576,-6.));
#12311=CARTESIAN_POINT('Ctrl Pts',(82.1373729617415,-24.826077429436,-6.));
#12312=CARTESIAN_POINT('Ctrl Pts',(82.0747258622901,-24.7849281529323,-6.));
#12313=CARTESIAN_POINT('Ctrl Pts',(82.0217931318391,-24.7501596867064,-6.));
#12314=CARTESIAN_POINT('Ctrl Pts',(81.9704561050628,-24.7128738527553,-6.));
#12315=CARTESIAN_POINT('Ctrl Pts',(81.9208801018963,-24.6732182969939,-6.));
#12316=CARTESIAN_POINT('Ctrl Pts',(81.8988503779666,-24.6555968493195,-6.));
#12317=CARTESIAN_POINT('Ctrl Pts',(81.877168685752,-24.6375073018008,-6.));
#12318=CARTESIAN_POINT('Ctrl Pts',(81.8558510844111,-24.6189618853867,-6.));
#12319=CARTESIAN_POINT('Ctrl Pts',(81.8441385439209,-24.6087724678633,-6.));
#12320=CARTESIAN_POINT('Ctrl Pts',(81.8325359306331,-24.5984454288214,-6.));
#12321=CARTESIAN_POINT('Ctrl Pts',(81.8210460423394,-24.5879827552104,-6.));
#12322=CARTESIAN_POINT('Ctrl Pts',(81.8104524505223,-24.5783362477147,-6.));
#12323=CARTESIAN_POINT('Ctrl Pts',(81.7999532489741,-24.5685729257818,-6.));
#12324=CARTESIAN_POINT('Ctrl Pts',(81.7895665184221,-24.5587098024996,-6.));
#12325=CARTESIAN_POINT('Ctrl Pts',(81.7364817644389,-24.5083011132282,-6.));
#12326=CARTESIAN_POINT('Ctrl Pts',(81.6862370051735,-24.4552040168816,-6.));
#12327=CARTESIAN_POINT('Ctrl Pts',(81.6390509066064,-24.3996779857533,-6.));
#12328=CARTESIAN_POINT('Ctrl Pts',(81.5922309432753,-24.3445828026317,-6.));
#12329=CARTESIAN_POINT('Ctrl Pts',(81.5484218497577,-24.2870953491844,-6.));
#12330=CARTESIAN_POINT('Ctrl Pts',(81.5078820330439,-24.2274448646231,-6.));
#12331=CARTESIAN_POINT('Ctrl Pts',(81.4741936202512,-24.1778755692962,-6.));
#12332=CARTESIAN_POINT('Ctrl Pts',(81.4427634629306,-24.1268119328391,-6.));
#12333=CARTESIAN_POINT('Ctrl Pts',(81.4137674499962,-24.0743790286647,-6.));
#12334=CARTESIAN_POINT('Ctrl Pts',(81.4016612987905,-24.052487720107,-6.));
#12335=CARTESIAN_POINT('Ctrl Pts',(81.3899797780391,-24.0303576880886,-6.));
#12336=CARTESIAN_POINT('Ctrl Pts',(81.3787371301748,-24.0079979523352,-6.));
#12337=CARTESIAN_POINT('Ctrl Pts',(81.3735363240541,-23.9976544236606,-6.));
#12338=CARTESIAN_POINT('Ctrl Pts',(81.3684294470406,-23.9872617395261,-6.));
#12339=CARTESIAN_POINT('Ctrl Pts',(81.3634179742616,-23.9768207948056,-6.));
#12340=CARTESIAN_POINT('Ctrl Pts',(81.358185972138,-23.9659203973858,-6.));
#12341=CARTESIAN_POINT('Ctrl Pts',(81.3530615649057,-23.9549748511129,-6.));
#12342=CARTESIAN_POINT('Ctrl Pts',(81.3480478111895,-23.9439894637078,-6.));
#12343=CARTESIAN_POINT('Ctrl Pts',(81.3195074050713,-23.881455993647,-6.));
#12344=CARTESIAN_POINT('Ctrl Pts',(81.2945279707571,-23.8175894738114,-6.));
#12345=CARTESIAN_POINT('Ctrl Pts',(81.273332967452,-23.7525943637814,-6.));
#12346=CARTESIAN_POINT('Ctrl Pts',(81.2541305056381,-23.6937094416857,-6.));
#12347=CARTESIAN_POINT('Ctrl Pts',(81.238034694834,-23.6338975545441,-6.));
#12348=CARTESIAN_POINT('Ctrl Pts',(81.2252484092018,-23.5733059254121,-6.));
#12349=CARTESIAN_POINT('Ctrl Pts',(81.2101158950681,-23.5015959925516,-6.));
#12350=CARTESIAN_POINT('Ctrl Pts',(81.199618304078,-23.4287923860598,-6.));
#12351=CARTESIAN_POINT('Ctrl Pts',(81.1936804986385,-23.3553182001535,-6.));
#12352=CARTESIAN_POINT('Ctrl Pts',(81.1923736703968,-23.3391475556011,-6.));
#12353=CARTESIAN_POINT('Ctrl Pts',(81.1912879323035,-23.3229445113856,-6.));
#12354=CARTESIAN_POINT('Ctrl Pts',(81.1904228526274,-23.3067137422975,-6.));
#12355=CARTESIAN_POINT('Ctrl Pts',(81.189527519046,-23.2899153443931,-6.));
#12356=CARTESIAN_POINT('Ctrl Pts',(81.1888685376905,-23.2730810540116,-6.));
#12357=CARTESIAN_POINT('Ctrl Pts',(81.1884459909198,-23.2562503281413,-6.));
#12358=CARTESIAN_POINT('Ctrl Pts',(81.1867247251221,-23.1876895088514,-6.));
#12359=CARTESIAN_POINT('Ctrl Pts',(81.1889150608861,-23.1191011358685,-6.));
#12360=CARTESIAN_POINT('Ctrl Pts',(81.1948964151315,-23.0508235285529,-6.));
#12361=CARTESIAN_POINT('Ctrl Pts',(81.2008765342427,-22.9825600203863,-6.));
#12362=CARTESIAN_POINT('Ctrl Pts',(81.2106465599838,-22.9146060779743,-6.));
#12363=CARTESIAN_POINT('Ctrl Pts',(81.2241355890059,-22.847314844313,-6.));
#12364=CARTESIAN_POINT('Ctrl Pts',(81.2338955811021,-22.79862624652,-6.));
#12365=CARTESIAN_POINT('Ctrl Pts',(81.2456036149723,-22.7502848589497,-6.));
#12366=CARTESIAN_POINT('Ctrl Pts',(81.2592470358225,-22.7024341008059,-6.));
#12367=CARTESIAN_POINT('Ctrl Pts',(81.2694833999489,-22.6665327099841,-6.));
#12368=CARTESIAN_POINT('Ctrl Pts',(81.2808094768484,-22.6309076580324,-6.));
#12369=CARTESIAN_POINT('Ctrl Pts',(81.2932238368812,-22.5956236937823,-6.));
#12370=CARTESIAN_POINT('Ctrl Pts',(81.297353318441,-22.5838869244811,-6.));
#12371=CARTESIAN_POINT('Ctrl Pts',(81.3016000214654,-22.5721970897154,-6.));
#12372=CARTESIAN_POINT('Ctrl Pts',(81.3059633013415,-22.5605567493468,-6.));
#12373=CARTESIAN_POINT('Ctrl Pts',(81.3290872411027,-22.498866796576,-6.));
#12374=CARTESIAN_POINT('Ctrl Pts',(81.3554837726698,-22.4385603794557,-6.));
#12375=CARTESIAN_POINT('Ctrl Pts',(81.3851029023407,-22.3799715846882,-6.));
#12376=CARTESIAN_POINT('Ctrl Pts',(81.4059352506056,-22.3387636832211,-6.));
#12377=CARTESIAN_POINT('Ctrl Pts',(81.4283626361963,-22.2984059990452,-6.));
#12378=CARTESIAN_POINT('Ctrl Pts',(81.4523780657584,-22.2590261197136,-6.));
#12379=CARTESIAN_POINT('Ctrl Pts',(81.460091074361,-22.2463785279948,-6.));
#12380=CARTESIAN_POINT('Ctrl Pts',(81.4679690461019,-22.233830189719,-6.));
#12381=CARTESIAN_POINT('Ctrl Pts',(81.4760084245406,-22.2213909668549,-6.));
#12382=CARTESIAN_POINT('Ctrl Pts',(81.5102529655807,-22.1684048459597,-6.));
#12383=CARTESIAN_POINT('Ctrl Pts',(81.547353278539,-22.1175025084971,-6.));
#12384=CARTESIAN_POINT('Ctrl Pts',(81.5872751269259,-22.0689991728902,-6.));
#12385=CARTESIAN_POINT('Ctrl Pts',(81.6240617830979,-22.0243049615181,-6.));
#12386=CARTESIAN_POINT('Ctrl Pts',(81.6632447942969,-21.9816476511376,-6.));
#12387=CARTESIAN_POINT('Ctrl Pts',(81.7048188123851,-21.9413067695052,-6.));
#12388=CARTESIAN_POINT('Ctrl Pts',(81.7126371595806,-21.9337203240935,-6.));
#12389=CARTESIAN_POINT('Ctrl Pts',(81.720540120158,-21.9262159047748,-6.));
#12390=CARTESIAN_POINT('Ctrl Pts',(81.7285261019851,-21.9187941775198,-6.));
#12391=CARTESIAN_POINT('Origin',(83.,-23.,-12.));
#12392=CARTESIAN_POINT('Origin',(83.,23.,-17.));
#12393=CARTESIAN_POINT('Ctrl Pts',(82.2300979593296,21.5225674811446,-17.));
#12394=CARTESIAN_POINT('Ctrl Pts',(82.2818391122695,21.4874949137045,-17.));
#12395=CARTESIAN_POINT('Ctrl Pts',(82.3355567543514,21.4556774402474,-17.));
#12396=CARTESIAN_POINT('Ctrl Pts',(82.3909195853492,21.4270510150662,-17.));
#12397=CARTESIAN_POINT('Ctrl Pts',(82.4260296219145,21.4088966899218,-17.));
#12398=CARTESIAN_POINT('Ctrl Pts',(82.4618022221282,21.3920264043057,-17.));
#12399=CARTESIAN_POINT('Ctrl Pts',(82.4981604879293,21.3764310360441,-17.));
#12400=CARTESIAN_POINT('Ctrl Pts',(82.5229436776791,21.3658006343369,-17.));
#12401=CARTESIAN_POINT('Ctrl Pts',(82.5479991038361,21.3557627158986,-17.));
#12402=CARTESIAN_POINT('Ctrl Pts',(82.5733036534702,21.3463159755545,-17.));
#12403=CARTESIAN_POINT('Ctrl Pts',(82.5867940813383,21.3412797045659,-17.));
#12404=CARTESIAN_POINT('Ctrl Pts',(82.6003552710179,21.3364116315714,-17.));
#12405=CARTESIAN_POINT('Ctrl Pts',(82.6139700106875,21.3317160828494,-17.));
#12406=CARTESIAN_POINT('Ctrl Pts',(82.6763343043471,21.3102074395331,-17.));
#12407=CARTESIAN_POINT('Ctrl Pts',(82.7398899091068,21.2922884683847,-17.));
#12408=CARTESIAN_POINT('Ctrl Pts',(82.8042869308727,21.2779126212872,-17.));
#12409=CARTESIAN_POINT('Ctrl Pts',(82.850739552613,21.2675426419139,-17.));
#12410=CARTESIAN_POINT('Ctrl Pts',(82.8976308987338,21.2590171252843,-17.));
#12411=CARTESIAN_POINT('Ctrl Pts',(82.9448387498772,21.252332630243,-17.));
#12412=CARTESIAN_POINT('Ctrl Pts',(82.9577364929077,21.2505063471726,-17.));
#12413=CARTESIAN_POINT('Ctrl Pts',(82.9706578945276,21.2488175569436,-17.));
#12414=CARTESIAN_POINT('Ctrl Pts',(82.9836005288407,21.2472663500385,-17.));
#12415=CARTESIAN_POINT('Ctrl Pts',(82.9969336049753,21.2456683477103,-17.));
#12416=CARTESIAN_POINT('Ctrl Pts',(83.010281297855,21.2442173442006,-17.));
#12417=CARTESIAN_POINT('Ctrl Pts',(83.0236353363373,21.2429134174335,-17.));
#12418=CARTESIAN_POINT('Ctrl Pts',(83.0911664964694,21.236319480519,-17.));
#12419=CARTESIAN_POINT('Ctrl Pts',(83.1589013412011,21.2334779274394,-17.));
#12420=CARTESIAN_POINT('Ctrl Pts',(83.2264851933794,21.2343408033929,-17.));
#12421=CARTESIAN_POINT('Ctrl Pts',(83.295047717335,21.2352161745257,-17.));
#12422=CARTESIAN_POINT('Ctrl Pts',(83.3634558539945,21.2399037043402,-17.));
#12423=CARTESIAN_POINT('Ctrl Pts',(83.4313607857131,21.2484016191192,-17.));
#12424=CARTESIAN_POINT('Ctrl Pts',(83.4734288208429,21.2536661937003,-17.));
#12425=CARTESIAN_POINT('Ctrl Pts',(83.5153040946816,21.2603941539428,-17.));
#12426=CARTESIAN_POINT('Ctrl Pts',(83.556905046585,21.2685950224746,-17.));
#12427=CARTESIAN_POINT('Ctrl Pts',(83.5909685001726,21.2753100107581,-17.));
#12428=CARTESIAN_POINT('Ctrl Pts',(83.6248480727517,21.2830126560453,-17.));
#12429=CARTESIAN_POINT('Ctrl Pts',(83.658498645678,21.2917121682308,-17.));
#12430=CARTESIAN_POINT('Ctrl Pts',(83.6722821813049,21.2952755558857,-17.));
#12431=CARTESIAN_POINT('Ctrl Pts',(83.686029760402,21.2990070804481,-17.));
#12432=CARTESIAN_POINT('Ctrl Pts',(83.6997150233873,21.3029005333424,-17.));
#12433=CARTESIAN_POINT('Ctrl Pts',(83.7675103738305,21.3221882886225,-17.));
#12434=CARTESIAN_POINT('Ctrl Pts',(83.833896115477,21.3454752233121,-17.));
#12435=CARTESIAN_POINT('Ctrl Pts',(83.8985095148681,21.372742621713,-17.));
#12436=CARTESIAN_POINT('Ctrl Pts',(83.905676412587,21.3757671128749,-17.));
#12437=CARTESIAN_POINT('Ctrl Pts',(83.912821512826,21.3788406285709,-17.));
#12438=CARTESIAN_POINT('Ctrl Pts',(83.9199443247218,21.3819631826297,-17.));
#12439=CARTESIAN_POINT('Ctrl Pts',(83.9816969964304,21.4090348024489,-17.));
#12440=CARTESIAN_POINT('Ctrl Pts',(84.0417752134862,21.4397880070069,-17.));
#12441=CARTESIAN_POINT('Ctrl Pts',(84.1000370416108,21.4739125980637,-17.));
#12442=CARTESIAN_POINT('Ctrl Pts',(84.1627128975786,21.5106225335889,-17.));
#12443=CARTESIAN_POINT('Ctrl Pts',(84.2232877181478,21.5512340617636,-17.));
#12444=CARTESIAN_POINT('Ctrl Pts',(84.2815649194341,21.595422083472,-17.));
#12445=CARTESIAN_POINT('Ctrl Pts',(84.2920904904965,21.6034029774122,-17.));
#12446=CARTESIAN_POINT('Ctrl Pts',(84.3025410380364,21.6115006876682,-17.));
#12447=CARTESIAN_POINT('Ctrl Pts',(84.3129152988056,21.619713487774,-17.));
#12448=CARTESIAN_POINT('Ctrl Pts',(84.3220910240519,21.626977465319,-17.));
#12449=CARTESIAN_POINT('Ctrl Pts',(84.3312000707531,21.6343259558301,-17.));
#12450=CARTESIAN_POINT('Ctrl Pts',(84.3402397897604,21.6417556641301,-17.));
#12451=CARTESIAN_POINT('Ctrl Pts',(84.3951430096276,21.6868803973225,-17.));
#12452=CARTESIAN_POINT('Ctrl Pts',(84.4475140924687,21.7350158683439,-17.));
#12453=CARTESIAN_POINT('Ctrl Pts',(84.4972030228202,21.7858120772864,-17.));
#12454=CARTESIAN_POINT('Ctrl Pts',(84.5479396850435,21.8376793659784,-17.));
#12455=CARTESIAN_POINT('Ctrl Pts',(84.595880656229,21.892321324379,-17.));
#12456=CARTESIAN_POINT('Ctrl Pts',(84.6408460217217,21.9494166317566,-17.));
#12457=CARTESIAN_POINT('Ctrl Pts',(84.6860841326239,22.0068582608603,-17.));
#12458=CARTESIAN_POINT('Ctrl Pts',(84.728311217856,22.0667838205659,-17.));
#12459=CARTESIAN_POINT('Ctrl Pts',(84.7673121163611,22.1289076492861,-17.));
#12460=CARTESIAN_POINT('Ctrl Pts',(84.7769392049,22.1442424652105,-17.));
#12461=CARTESIAN_POINT('Ctrl Pts',(84.7863695336446,22.1597113916503,-17.));
#12462=CARTESIAN_POINT('Ctrl Pts',(84.7955994818445,22.1753104375009,-17.));
#12463=CARTESIAN_POINT('Ctrl Pts',(84.8028490082894,22.1875624775946,-17.));
#12464=CARTESIAN_POINT('Ctrl Pts',(84.8099756566119,22.1998963399229,-17.));
#12465=CARTESIAN_POINT('Ctrl Pts',(84.8169672073596,22.2122910124967,-17.));
#12466=CARTESIAN_POINT('Ctrl Pts',(84.8539823502387,22.2779117299617,-17.));
#12467=CARTESIAN_POINT('Ctrl Pts',(84.8872834125653,22.3453494005186,-17.));
#12468=CARTESIAN_POINT('Ctrl Pts',(84.9166896640119,22.414257705163,-17.));
#12469=CARTESIAN_POINT('Ctrl Pts',(84.946127984178,22.4832411571309,-17.));
#12470=CARTESIAN_POINT('Ctrl Pts',(84.9716637589054,22.5536992817437,-17.));
#12471=CARTESIAN_POINT('Ctrl Pts',(84.9930799285708,22.6253223370055,-17.));
#12472=CARTESIAN_POINT('Ctrl Pts',(85.014008872031,22.6953159398509,-17.));
#12473=CARTESIAN_POINT('Ctrl Pts',(85.0310040806236,22.7664229483095,-17.));
#12474=CARTESIAN_POINT('Ctrl Pts',(85.0438193705755,22.8383774944687,-17.));
#12475=CARTESIAN_POINT('Ctrl Pts',(85.0465681840663,22.8538113729024,-17.));
#12476=CARTESIAN_POINT('Ctrl Pts',(85.0491245073901,22.8692843043202,-17.));
#12477=CARTESIAN_POINT('Ctrl Pts',(85.0514856033279,22.8847937492575,-17.));
#12478=CARTESIAN_POINT('Ctrl Pts',(85.0534987896279,22.8980178633515,-17.));
#12479=CARTESIAN_POINT('Ctrl Pts',(85.0553700412629,22.9112685237034,-17.));
#12480=CARTESIAN_POINT('Ctrl Pts',(85.0571001857713,22.9245440319506,-17.));
#12481=CARTESIAN_POINT('Ctrl Pts',(84.8174278887595,23.9586205879593,-17.));
#12482=CARTESIAN_POINT('Ctrl Pts',(84.7765814369624,24.021100311179,-17.));
#12483=CARTESIAN_POINT('Ctrl Pts',(84.7321382857191,24.0810293094923,-17.));
#12484=CARTESIAN_POINT('Ctrl Pts',(84.6844272864798,24.1382578115838,-17.));
#12485=CARTESIAN_POINT('Ctrl Pts',(84.6379676938528,24.1939852735153,-17.));
#12486=CARTESIAN_POINT('Ctrl Pts',(84.5884084330975,24.2471522504166,-17.));
#12487=CARTESIAN_POINT('Ctrl Pts',(84.5360270889349,24.2975827793496,-17.));
#12488=CARTESIAN_POINT('Ctrl Pts',(84.524335411062,24.3088390292354,-17.));
#12489=CARTESIAN_POINT('Ctrl Pts',(84.5125014719912,24.3199602485304,-17.));
#12490=CARTESIAN_POINT('Ctrl Pts',(84.5005333434906,24.3309395401516,-17.));
#12491=CARTESIAN_POINT('Ctrl Pts',(84.4456121081234,24.3813230449125,-17.));
#12492=CARTESIAN_POINT('Ctrl Pts',(84.3879771334341,24.4286220664064,-17.));
#12493=CARTESIAN_POINT('Ctrl Pts',(84.3279445697082,24.4726641188265,-17.));
#12494=CARTESIAN_POINT('Ctrl Pts',(84.2858000274712,24.5035828739691,-17.));
#12495=CARTESIAN_POINT('Ctrl Pts',(84.2424731669021,24.5328955590232,-17.));
#12496=CARTESIAN_POINT('Ctrl Pts',(84.1980680473418,24.5605280932164,-17.));
#12497=CARTESIAN_POINT('Ctrl Pts',(84.1811926620229,24.5710293522259,-17.));
#12498=CARTESIAN_POINT('Ctrl Pts',(84.1641615210443,24.5812878268755,-17.));
#12499=CARTESIAN_POINT('Ctrl Pts',(84.1469802604654,24.5912989639673,-17.));
#12500=CARTESIAN_POINT('Ctrl Pts',(84.1305954137665,24.6008460484653,-17.));
#12501=CARTESIAN_POINT('Ctrl Pts',(84.1140687260479,24.6101709300663,-17.));
#12502=CARTESIAN_POINT('Ctrl Pts',(84.0974346776955,24.6192537517685,-17.));
#12503=CARTESIAN_POINT('Ctrl Pts',(84.0337176308478,24.6540456775616,-17.));
#12504=CARTESIAN_POINT('Ctrl Pts',(83.968361627354,24.6853304511806,-17.));
#12505=CARTESIAN_POINT('Ctrl Pts',(83.9016583718977,24.7129464384693,-17.));
#12506=CARTESIAN_POINT('Ctrl Pts',(83.8363874432689,24.7399694244241,-17.));
#12507=CARTESIAN_POINT('Ctrl Pts',(83.7698255763795,24.7634796468367,-17.));
#12508=CARTESIAN_POINT('Ctrl Pts',(83.7022374818724,24.7832774030826,-17.));
#12509=CARTESIAN_POINT('Ctrl Pts',(83.6361317195128,24.8026409578506,-17.));
#12510=CARTESIAN_POINT('Ctrl Pts',(83.5690434882077,24.818453214359,-17.));
#12511=CARTESIAN_POINT('Ctrl Pts',(83.501224394617,24.8304787382213,-17.));
#12512=CARTESIAN_POINT('Ctrl Pts',(83.4791642918285,24.8343903843144,-17.));
#12513=CARTESIAN_POINT('Ctrl Pts',(83.4570269381163,24.8379009736306,-17.));
#12514=CARTESIAN_POINT('Ctrl Pts',(83.4348212870326,24.8410012299466,-17.));
#12515=CARTESIAN_POINT('Ctrl Pts',(83.4223367367169,24.8427442685012,-17.));
#12516=CARTESIAN_POINT('Ctrl Pts',(83.4098293128072,24.8443576459882,-17.));
#12517=CARTESIAN_POINT('Ctrl Pts',(83.3973183107669,24.8458378344555,-17.));
#12518=CARTESIAN_POINT('Ctrl Pts',(83.3294876076222,24.8538629490063,-17.));
#12519=CARTESIAN_POINT('Ctrl Pts',(83.2614333839518,24.857994846758,-17.));
#12520=CARTESIAN_POINT('Ctrl Pts',(83.1934013670207,24.8580554883464,-17.));
#12521=CARTESIAN_POINT('Ctrl Pts',(83.1836044640327,24.8580642209959,-17.));
#12522=CARTESIAN_POINT('Ctrl Pts',(83.1738080277562,24.8579884388901,-17.));
#12523=CARTESIAN_POINT('Ctrl Pts',(83.1640128014146,24.8578275203802,-17.));
#12524=CARTESIAN_POINT('Ctrl Pts',(83.0946485636743,24.8566879867553,-17.));
#12525=CARTESIAN_POINT('Ctrl Pts',(83.0253435429726,24.8512831792143,-17.));
#12526=CARTESIAN_POINT('Ctrl Pts',(82.9564227427862,24.8417863242814,-17.));
#12527=CARTESIAN_POINT('Ctrl Pts',(82.892127503802,24.8329268427337,-17.));
#12528=CARTESIAN_POINT('Ctrl Pts',(82.8281661293059,24.8205052274388,-17.));
#12529=CARTESIAN_POINT('Ctrl Pts',(82.7648229902021,24.8046276724132,-17.));
#12530=CARTESIAN_POINT('Ctrl Pts',(82.7509583247458,24.8011523632982,-17.));
#12531=CARTESIAN_POINT('Ctrl Pts',(82.7371233769276,24.7975113717667,-17.));
#12532=CARTESIAN_POINT('Ctrl Pts',(82.7233213065985,24.7937056333022,-17.));
#12533=CARTESIAN_POINT('Ctrl Pts',(82.712260901116,24.7906558726812,-17.));
#12534=CARTESIAN_POINT('Ctrl Pts',(82.7012221546017,24.7875003763038,-17.));
#12535=CARTESIAN_POINT('Ctrl Pts',(82.6902197481713,24.7842437511852,-17.));
#12536=CARTESIAN_POINT('Ctrl Pts',(82.6246575930502,24.7648378727943,-17.));
#12537=CARTESIAN_POINT('Ctrl Pts',(82.5602618201431,24.7418119987196,-17.));
#12538=CARTESIAN_POINT('Ctrl Pts',(82.4973348852617,24.715348146897,-17.));
#12539=CARTESIAN_POINT('Ctrl Pts',(82.4346992973391,24.6890068207108,-17.));
#12540=CARTESIAN_POINT('Ctrl Pts',(82.3735180853771,24.6592585759547,-17.));
#12541=CARTESIAN_POINT('Ctrl Pts',(82.3141193166054,24.626241363502,-17.));
#12542=CARTESIAN_POINT('Ctrl Pts',(82.2559932421632,24.5939315869093,-17.));
#12543=CARTESIAN_POINT('Ctrl Pts',(82.1995733746079,24.5584907230117,-17.));
#12544=CARTESIAN_POINT('Ctrl Pts',(82.1452070792864,24.5200186444709,-17.));
#12545=CARTESIAN_POINT('Ctrl Pts',(82.1337105081942,24.5118831446471,-17.));
#12546=CARTESIAN_POINT('Ctrl Pts',(82.1223059328567,24.5036120109462,-17.));
#12547=CARTESIAN_POINT('Ctrl Pts',(82.1109969163345,24.4952060590793,-17.));
#12548=CARTESIAN_POINT('Ctrl Pts',(82.1003659149212,24.4873040734378,-17.));
#12549=CARTESIAN_POINT('Ctrl Pts',(82.0898181260854,24.4792818391566,-17.));
#12550=CARTESIAN_POINT('Ctrl Pts',(82.0793730883428,24.4711532945118,-17.));
#12551=CARTESIAN_POINT('Ctrl Pts',(82.0278057382619,24.4310225149325,-17.));
#12552=CARTESIAN_POINT('Ctrl Pts',(81.9786449613375,24.388234245707,-17.));
#12553=CARTESIAN_POINT('Ctrl Pts',(81.9321818346833,24.3429204973124,-17.));
#12554=CARTESIAN_POINT('Ctrl Pts',(81.8866023381703,24.2984685203218,-17.));
#12555=CARTESIAN_POINT('Ctrl Pts',(81.8436182780009,24.2515855470076,-17.));
#12556=CARTESIAN_POINT('Ctrl Pts',(81.8035469551829,24.2023704370989,-17.));
#12557=CARTESIAN_POINT('Ctrl Pts',(81.7647767394068,24.1547533309887,-17.));
#12558=CARTESIAN_POINT('Ctrl Pts',(81.7287328388918,24.1049525046523,-17.));
#12559=CARTESIAN_POINT('Ctrl Pts',(81.6957493048722,24.0530421344184,-17.));
#12560=CARTESIAN_POINT('Ctrl Pts',(81.6902970764157,24.0444612710819,-17.));
#12561=CARTESIAN_POINT('Ctrl Pts',(81.6849285841721,24.035822741006,-17.));
#12562=CARTESIAN_POINT('Ctrl Pts',(81.6796454747864,24.0271268532951,-17.));
#12563=CARTESIAN_POINT('Ctrl Pts',(81.6739898969948,24.0178178903669,-17.));
#12564=CARTESIAN_POINT('Ctrl Pts',(81.6684321663704,24.0084431960771,-17.));
#12565=CARTESIAN_POINT('Ctrl Pts',(81.6629726863575,23.9990044309052,-17.));
#12566=CARTESIAN_POINT('Origin',(83.,23.,-4.45407471946233));
#12567=CARTESIAN_POINT('Ctrl Pts',(80.9434277056327,23.0014963838888,-6.20407471946233));
#12568=CARTESIAN_POINT('Ctrl Pts',(80.942610779565,23.0996693924379,-6.20941233124781));
#12569=CARTESIAN_POINT('Ctrl Pts',(80.9936360048529,23.8783594097717,-6.25179431569715));
#12570=CARTESIAN_POINT('Ctrl Pts',(81.9885904398633,25.2081812989956,-6.33122067281032));
#12571=CARTESIAN_POINT('Ctrl Pts',(84.3064562032972,25.0471892646279,-6.44235379080189));
#12572=CARTESIAN_POINT('Ctrl Pts',(85.4285783999577,23.0128601032299,-6.55348690879345));
#12573=CARTESIAN_POINT('Ctrl Pts',(84.3279818049202,20.9665948756778,-6.664620026785));
#12574=CARTESIAN_POINT('Ctrl Pts',(82.0119581026862,20.781465281165,-6.77575314477657));
#12575=CARTESIAN_POINT('Ctrl Pts',(80.9980257384601,22.1068136403803,-6.855571375669));
#12576=CARTESIAN_POINT('Ctrl Pts',(80.9427191451532,22.892962770366,-6.89834523389759));
#12577=CARTESIAN_POINT('Ctrl Pts',(80.943624771683,22.9983937941554,-6.90407471946232));
#12578=CARTESIAN_POINT('Ctrl Pts',(80.9473274657881,22.9976809234163,-6.14592528053767));
#12579=CARTESIAN_POINT('Ctrl Pts',(80.9508754982181,23.4678290021184,-6.17137226568616));
#12580=CARTESIAN_POINT('Ctrl Pts',(81.3433671991295,24.6294006980789,-6.23386362349849));
#12581=CARTESIAN_POINT('Ctrl Pts',(83.2718171861771,25.4128332182024,-6.33339935397467));
#12582=CARTESIAN_POINT('Ctrl Pts',(85.1745320403748,24.0812968093214,-6.44453247196624));
#12583=CARTESIAN_POINT('Ctrl Pts',(85.0878555272437,21.7590837146758,-6.55566558995779));
#12584=CARTESIAN_POINT('Ctrl Pts',(83.0898774457969,20.5731226537472,-6.66679870794935));
#12585=CARTESIAN_POINT('Ctrl Pts',(81.2789896272084,21.4741601405839,-6.76355193814265));
#12586=CARTESIAN_POINT('Ctrl Pts',(80.9500836416261,22.5818790379909,-6.82326079567209));
#12587=CARTESIAN_POINT('Ctrl Pts',(80.9479086080167,23.0011644845222,-6.84592528053768));
#12588=CARTESIAN_POINT('Ctrl Pts',(84.2690708798524,24.0793586530485,-6.));
#12589=CARTESIAN_POINT('Ctrl Pts',(84.627967898288,23.6573805147568,-6.03704437266385));
#12590=CARTESIAN_POINT('Ctrl Pts',(84.8852386427553,22.4342554940614,-6.11113311799156));
#12591=CARTESIAN_POINT('Ctrl Pts',(83.5452631709912,21.1066470201579,-6.22226623598311));
#12592=CARTESIAN_POINT('Ctrl Pts',(81.705991976553,21.516300728788,-6.33339935397468));
#12593=CARTESIAN_POINT('Ctrl Pts',(81.0511940873356,23.2817532913239,-6.44453247196623));
#12594=CARTESIAN_POINT('Ctrl Pts',(82.1799448462403,24.7904027468678,-6.5556655899578));
#12595=CARTESIAN_POINT('Ctrl Pts',(84.0592802212889,24.6598697237475,-6.66679870794935));
#12596=CARTESIAN_POINT('Ctrl Pts',(84.9691016495094,23.0104270261496,-6.77793182594091));
#12597=CARTESIAN_POINT('Ctrl Pts',(84.0767332702261,21.3513065155757,-6.88906494393247));
#12598=CARTESIAN_POINT('Ctrl Pts',(82.1988914461979,21.201202656489,-7.00019806192403));
#12599=CARTESIAN_POINT('Ctrl Pts',(81.0542580966476,22.697395090279,-7.11133117991559));
#12600=CARTESIAN_POINT('Ctrl Pts',(81.6904431199867,24.4705604132256,-7.22246429790715));
#12601=CARTESIAN_POINT('Ctrl Pts',(83.5251867456106,24.8978024588301,-7.33359741589872));
#12602=CARTESIAN_POINT('Ctrl Pts',(84.8792584886388,23.5881052624922,-7.44473053389026));
#12603=CARTESIAN_POINT('Ctrl Pts',(84.5133590473266,21.7401488437674,-7.55586365188183));
#12604=CARTESIAN_POINT('Ctrl Pts',(82.7623737647797,21.0452588627609,-7.66699676987339));
#12605=CARTESIAN_POINT('Ctrl Pts',(81.2288734036351,22.139424370776,-7.77812988786495));
#12606=CARTESIAN_POINT('Ctrl Pts',(81.3163777952684,24.0212228361577,-7.8892630058565));
#12607=CARTESIAN_POINT('Ctrl Pts',(82.9447995049623,24.9683578317838,-8.00039612384807));
#12608=CARTESIAN_POINT('Ctrl Pts',(84.6237428755888,24.113974333724,-8.11152924183962));
#12609=CARTESIAN_POINT('Ctrl Pts',(84.8165728589842,22.2400376458565,-8.22266235983118));
#12610=CARTESIAN_POINT('Ctrl Pts',(83.3468038610209,21.061648433366,-8.33379547782274));
#12611=CARTESIAN_POINT('Ctrl Pts',(81.5596263199885,21.6573148588903,-8.4449285958143));
#12612=CARTESIAN_POINT('Ctrl Pts',(81.0907354631553,23.4818595774137,-8.55606171380585));
#12613=CARTESIAN_POINT('Ctrl Pts',(82.3692786585142,24.8653874427323,-8.66719483179742));
#12614=CARTESIAN_POINT('Ctrl Pts',(84.2250828504748,24.5416393006048,-8.77832794978898));
#12615=CARTESIAN_POINT('Ctrl Pts',(84.959642998928,22.8069221916923,-8.88946106778053));
#12616=CARTESIAN_POINT('Ctrl Pts',(83.9006607439461,21.2489174926821,-9.00059418577209));
#12617=CARTESIAN_POINT('Ctrl Pts',(82.0173583264533,21.2935724261695,-9.11172730376366));
#12618=CARTESIAN_POINT('Ctrl Pts',(81.0334082449847,22.9000170396293,-9.22286042175521));
#12619=CARTESIAN_POINT('Ctrl Pts',(81.8493603420058,24.5979699936773,-9.33399353974677));
#12620=CARTESIAN_POINT('Ctrl Pts',(83.7184231427578,24.8333979140429,-9.44512665773834));
#12621=CARTESIAN_POINT('Ctrl Pts',(84.9299568063988,23.3908279016291,-9.55625977572989));
#12622=CARTESIAN_POINT('Ctrl Pts',(84.375118038464,21.5905568108124,-9.66739289372145));
#12623=CARTESIAN_POINT('Ctrl Pts',(82.5617171176083,21.0802636018814,-9.77852601171301));
#12624=CARTESIAN_POINT('Ctrl Pts',(81.1494499413637,22.3269887045979,-9.88965912970457));
#12625=CARTESIAN_POINT('Ctrl Pts',(81.4308790157235,24.1896802343324,-10.0007922476961));
#12626=CARTESIAN_POINT('Ctrl Pts',(83.1484293748935,24.9635295882484,-10.1119253656877));
#12627=CARTESIAN_POINT('Ctrl Pts',(84.7301313280375,23.9402793792279,-10.2230584836792));
#12628=CARTESIAN_POINT('Ctrl Pts',(84.7283489924563,22.0564484733023,-10.3341916016708));
#12629=CARTESIAN_POINT('Ctrl Pts',(83.1447136318255,21.0361930624367,-10.4453247196624));
#12630=CARTESIAN_POINT('Ctrl Pts',(81.4286306594752,21.8132910555169,-10.5564578376539));
#12631=CARTESIAN_POINT('Ctrl Pts',(81.1507267560675,23.6765117829969,-10.6675909556455));
#12632=CARTESIAN_POINT('Ctrl Pts',(82.5653505121927,24.9205622994339,-10.778724073637));
#12633=CARTESIAN_POINT('Ctrl Pts',(84.3777825871961,24.4068386068335,-10.8898571916286));
#12634=CARTESIAN_POINT('Ctrl Pts',(84.9292138094035,22.6055208486311,-11.0009903096202));
#12635=CARTESIAN_POINT('Ctrl Pts',(83.7149526201293,21.1652459363096,-11.1121234276117));
#12636=CARTESIAN_POINT('Ctrl Pts',(81.8463386526518,21.4042101582938,-11.2232565456033));
#12637=CARTESIAN_POINT('Ctrl Pts',(81.0336009579355,23.1037040530836,-11.3343896635948));
#12638=CARTESIAN_POINT('Ctrl Pts',(82.0205890632288,24.7082839167396,-11.4455227815864));
#12639=CARTESIAN_POINT('Ctrl Pts',(83.9039726070939,24.7493751023956,-11.5566558995779));
#12640=CARTESIAN_POINT('Ctrl Pts',(84.9600048409316,23.1893693396062,-11.6677890175695));
#12641=CARTESIAN_POINT('Ctrl Pts',(84.2221634993099,21.4560453037046,-11.7789221355611));
#12642=CARTESIAN_POINT('Ctrl Pts',(82.3657500192332,21.1358093753172,-11.8900552535526));
#12643=CARTESIAN_POINT('Ctrl Pts',(81.0898270853904,22.5217540804675,-12.0011883715442));
#12644=CARTESIAN_POINT('Ctrl Pts',(81.5621695866715,24.3454082747499,-12.1123214895357));
#12645=CARTESIAN_POINT('Ctrl Pts',(83.3504710746846,24.9376918612276,-12.2234546075273));
#12646=CARTESIAN_POINT('Ctrl Pts',(84.8180076407391,23.7565235895013,-12.3345877255189));
#12647=CARTESIAN_POINT('Ctrl Pts',(84.621632057906,21.8829551521851,-12.4457208435104));
#12648=CARTESIAN_POINT('Ctrl Pts',(82.9410749888612,21.0317501260459,-12.556853961502));
#12649=CARTESIAN_POINT('Ctrl Pts',(81.3144484092768,21.9819648541096,-12.6679870794936));
#12650=CARTESIAN_POINT('Ctrl Pts',(81.2305049881862,23.8639254171651,-12.7791201974851));
#12651=CARTESIAN_POINT('Ctrl Pts',(82.7660730485526,24.955187434658,-12.8902533154767));
#12652=CARTESIAN_POINT('Ctrl Pts',(84.5157402621589,24.2569849565244,-13.0013864334682));
#12653=CARTESIAN_POINT('Ctrl Pts',(84.8781423288819,22.4083403717338,-13.1125195514598));
#12654=CARTESIAN_POINT('Ctrl Pts',(83.5215946132505,21.1012059662286,-13.2236526694514));
#12655=CARTESIAN_POINT('Ctrl Pts',(81.6876629778084,21.5319225962357,-13.3347857874429));
#12656=CARTESIAN_POINT('Ctrl Pts',(81.0548338381576,23.3062814491317,-13.4459189054345));
#12657=CARTESIAN_POINT('Ctrl Pts',(82.2022973308199,24.8003194646615,-13.557052023426));
#12658=CARTESIAN_POINT('Ctrl Pts',(84.079849703585,24.6466342462504,-13.6681851414176));
#12659=CARTESIAN_POINT('Ctrl Pts',(84.969081125163,22.9858845547767,-13.7793182594091));
#12660=CARTESIAN_POINT('Ctrl Pts',(84.056131998706,21.3380538743536,-13.8904513774007));
#12661=CARTESIAN_POINT('Ctrl Pts',(82.1765692980985,21.2113017016767,-14.0015844953923));
#12662=CARTESIAN_POINT('Ctrl Pts',(81.0506427857571,22.7216366141191,-14.1127176133838));
#12663=CARTESIAN_POINT('Ctrl Pts',(81.7088447219042,24.4867406535661,-14.2238507313754));
#12664=CARTESIAN_POINT('Ctrl Pts',(83.5487627878191,24.8911211293868,-14.3349838493669));
#12665=CARTESIAN_POINT('Ctrl Pts',(84.8864315514728,23.564673113672,-14.4461169673585));
#12666=CARTESIAN_POINT('Ctrl Pts',(84.4975639095097,21.7214140392435,-14.5572500853501));
#12667=CARTESIAN_POINT('Ctrl Pts',(82.7380668349932,21.0483671602815,-14.6683832033416));
#12668=CARTESIAN_POINT('Ctrl Pts',(81.2183013007427,22.161531472689,-14.7795163213332));
#12669=CARTESIAN_POINT('Ctrl Pts',(81.329216546894,24.0420951812183,-14.8906494393247));
#12670=CARTESIAN_POINT('Ctrl Pts',(82.9692985630169,24.9688923671652,-15.0017825573163));
#12671=CARTESIAN_POINT('Ctrl Pts',(84.6374797580343,24.0936817563847,-15.1129156753079));
#12672=CARTESIAN_POINT('Ctrl Pts',(84.806974997268,22.2174905701235,-15.2240487932994));
#12673=CARTESIAN_POINT('Ctrl Pts',(83.3226556582986,21.0574827837253,-15.335181911291));
#12674=CARTESIAN_POINT('Ctrl Pts',(81.5430290393143,21.6753432694906,-15.4463150292825));
#12675=CARTESIAN_POINT('Ctrl Pts',(81.0968798325604,23.5055816151367,-15.5574481472741));
#12676=CARTESIAN_POINT('Ctrl Pts',(82.3925406241014,24.8730920021767,-15.6685812652657));
#12677=CARTESIAN_POINT('Ctrl Pts',(84.2441731131724,24.526274395825,-15.7797143832572));
#12678=CARTESIAN_POINT('Ctrl Pts',(84.9570874696211,22.7825513238517,-15.8908475012488));
#12679=CARTESIAN_POINT('Ctrl Pts',(83.8788021914142,21.2378439741891,-16.0019806192403));
#12680=CARTESIAN_POINT('Ctrl Pts',(81.996194884314,21.3059348963008,-16.1131137372319));
#12681=CARTESIAN_POINT('Ctrl Pts',(81.0323248335547,22.9244934615319,-16.2242468552234));
#12682=CARTESIAN_POINT('Ctrl Pts',(81.8693180174765,24.6121733762817,-16.335379973215));
#12683=CARTESIAN_POINT('Ctrl Pts',(83.7412167335509,24.8242992580383,-16.4465130912066));
#12684=CARTESIAN_POINT('Ctrl Pts',(84.9346033040057,23.3668134991485,-16.5576462091981));
#12685=CARTESIAN_POINT('Ctrl Pts',(84.3576069455347,21.5734882290582,-16.6687793271897));
#12686=CARTESIAN_POINT('Ctrl Pts',(82.5375922462901,21.0859967419785,-16.7799124451812));
#12687=CARTESIAN_POINT('Ctrl Pts',(81.1417554914442,22.349809536703,-16.8910455631728));
#12688=CARTESIAN_POINT('Ctrl Pts',(81.4447236992157,24.2096334404004,-17.0021786811644));
#12689=CARTESIAN_POINT('Ctrl Pts',(83.1751260846232,24.9604903571868,-17.1133117991559));
#12690=CARTESIAN_POINT('Ctrl Pts',(84.2151340020225,24.2672324081111,-17.1874005444836));
#12691=CARTESIAN_POINT('Ctrl Pts',(84.4735782273626,23.7772536316049,-17.2244449171475));
#12692=CARTESIAN_POINT('Ctrl Pts',(84.3677806246588,24.1633123698098,-5.92518502761751));
#12693=CARTESIAN_POINT('Ctrl Pts',(84.7545930524416,23.7085123024942,-5.96222940028136));
#12694=CARTESIAN_POINT('Ctrl Pts',(85.0318746016131,22.3902512570299,-6.03631814560907));
#12695=CARTESIAN_POINT('Ctrl Pts',(83.5876743470062,20.9593799191348,-6.14745126360063));
#12696=CARTESIAN_POINT('Ctrl Pts',(81.6053425929765,21.4008969489394,-6.25858438159219));
#12697=CARTESIAN_POINT('Ctrl Pts',(80.8996137955093,23.3036683757581,-6.36971749958375));
#12698=CARTESIAN_POINT('Ctrl Pts',(82.1161600441146,24.9296622642438,-6.48085061757531));
#12699=CARTESIAN_POINT('Ctrl Pts',(84.1416722152917,24.7889762373743,-6.59198373556687));
#12700=CARTESIAN_POINT('Ctrl Pts',(85.1222605663254,23.011238051843,-6.70311685355843));
#12701=CARTESIAN_POINT('Ctrl Pts',(84.1604827817908,21.2230693022764,-6.81424997154998));
#12702=CARTESIAN_POINT('Ctrl Pts',(82.136580331694,21.0612901980477,-6.92538308954154));
#12703=CARTESIAN_POINT('Ctrl Pts',(80.9029161268739,22.6738581437696,-7.0365162075331));
#12704=CARTESIAN_POINT('Ctrl Pts',(81.5885843290494,24.5849422380838,-7.14764932552467));
#12705=CARTESIAN_POINT('Ctrl Pts',(83.5660363549255,25.0454156452787,-7.25878244351622));
#12706=CARTESIAN_POINT('Ctrl Pts',(85.0254293044568,23.6338487440436,-7.36991556150778));
#12707=CARTESIAN_POINT('Ctrl Pts',(84.6310697975563,21.6421562193206,-7.48104867949934));
#12708=CARTESIAN_POINT('Ctrl Pts',(82.7438909318581,20.8932169225645,-7.5921817974909));
#12709=CARTESIAN_POINT('Ctrl Pts',(81.091113206689,22.0724878409919,-7.70331491548246));
#12710=CARTESIAN_POINT('Ctrl Pts',(81.1854237872472,24.1006546844083,-7.81444803347401));
#12711=CARTESIAN_POINT('Ctrl Pts',(82.9405059490508,25.1214588936298,-7.92558115146558));
#12712=CARTESIAN_POINT('Ctrl Pts',(84.7500394027767,24.2006204966362,-8.03671426945713));
#12713=CARTESIAN_POINT('Ctrl Pts',(84.9578679167935,22.1809269285348,-8.14784738744869));
#12714=CARTESIAN_POINT('Ctrl Pts',(83.3737786511311,20.9108812922038,-8.25898050544026));
#12715=CARTESIAN_POINT('Ctrl Pts',(81.4475924528209,21.5528793149514,-8.37011362343181));
#12716=CARTESIAN_POINT('Ctrl Pts',(80.9422307435277,23.5193391513873,-8.48124674142336));
#12717=CARTESIAN_POINT('Ctrl Pts',(82.3202204509307,25.0104793531689,-8.59237985941493));
#12718=CARTESIAN_POINT('Ctrl Pts',(84.3203711574219,24.6615497203948,-8.70351297740649));
#12719=CARTESIAN_POINT('Ctrl Pts',(85.1120662113796,22.7919043849736,-8.81464609539804));
#12720=CARTESIAN_POINT('Ctrl Pts',(83.9707151385458,21.11271634728,-8.9257792133896));
#12721=CARTESIAN_POINT('Ctrl Pts',(81.94092736395,21.1608445911701,-9.03691233138117));
#12722=CARTESIAN_POINT('Ctrl Pts',(80.8804445505544,22.8922402537462,-9.14804544937273));
#12723=CARTESIAN_POINT('Ctrl Pts',(81.7598623093837,24.7222618774392,-9.25917856736428));
#12724=CARTESIAN_POINT('Ctrl Pts',(83.7743028940076,24.9760016433514,-9.37031168535585));
#12725=CARTESIAN_POINT('Ctrl Pts',(85.0800709937715,23.4212269305923,-9.4814448033474));
#12726=CARTESIAN_POINT('Ctrl Pts',(84.4820762492386,21.4809287516294,-9.59257792133897));
#12727=CARTESIAN_POINT('Ctrl Pts',(82.5276269874504,20.9309443692346,-9.70371103933052));
#12728=CARTESIAN_POINT('Ctrl Pts',(81.0055120991678,22.2746411373535,-9.81484415732209));
#12729=CARTESIAN_POINT('Ctrl Pts',(81.3088310400058,24.2822148864126,-9.92597727531363));
#12730=CARTESIAN_POINT('Ctrl Pts',(83.1599743767922,25.116255103941,-10.0371103933052));
#12731=CARTESIAN_POINT('Ctrl Pts',(84.8647028674081,24.0134153553533,-10.1482435112968));
#12732=CARTESIAN_POINT('Ctrl Pts',(84.8627818997827,21.9830579859066,-10.2593766292883));
#12733=CARTESIAN_POINT('Ctrl Pts',(83.1559696190948,20.8834459742058,-10.3705097472799));
#12734=CARTESIAN_POINT('Ctrl Pts',(81.3064078041073,21.7209875136666,-10.4816428652714));
#12735=CARTESIAN_POINT('Ctrl Pts',(81.0068882259397,23.7291316220605,-10.592775983263));
#12736=CARTESIAN_POINT('Ctrl Pts',(82.5315429915074,25.0699457716037,-10.7039091012546));
#12737=CARTESIAN_POINT('Ctrl Pts',(84.4849480495354,24.5162640787035,-10.8150422192461));
#12738=CARTESIAN_POINT('Ctrl Pts',(85.0792702056432,22.5748378214013,-10.9261753372377));
#12739=CARTESIAN_POINT('Ctrl Pts',(83.7705624302684,21.0225367241728,-11.0373084552292));
#12740=CARTESIAN_POINT('Ctrl Pts',(81.7566055896702,21.2800878491775,-11.1484415732208));
#12741=CARTESIAN_POINT('Ctrl Pts',(80.880652252933,23.1117702696975,-11.2595746912123));
#12742=CARTESIAN_POINT('Ctrl Pts',(81.944409391026,24.8411561401554,-11.3707078092039));
#12743=CARTESIAN_POINT('Ctrl Pts',(83.9742846020934,24.8854434439435,-11.4818409271955));
#12744=CARTESIAN_POINT('Ctrl Pts',(85.1124561978568,23.2040986975037,-11.592974045187));
#12745=CARTESIAN_POINT('Ctrl Pts',(84.3172247358758,21.3359547898621,-11.7041071631786));
#12746=CARTESIAN_POINT('Ctrl Pts',(82.3164173501609,20.9908105547198,-11.8152402811701));
#12747=CARTESIAN_POINT('Ctrl Pts',(80.9412517111298,22.484555580824,-11.9263733991617));
#12748=CARTESIAN_POINT('Ctrl Pts',(81.4503335376155,24.4500556270526,-12.0375065171532));
#12749=CARTESIAN_POINT('Ctrl Pts',(83.3777311047534,25.0884076897694,-12.1486396351448));
#12750=CARTESIAN_POINT('Ctrl Pts',(84.9594142974693,23.8153668358835,-12.2597727531364));
#12751=CARTESIAN_POINT('Ctrl Pts',(84.7477644033464,21.7960701612711,-12.3709058711279));
#12752=CARTESIAN_POINT('Ctrl Pts',(82.936491735944,20.8786574612801,-12.4820389891195));
#12753=CARTESIAN_POINT('Ctrl Pts',(81.1833443314669,21.9027809479542,-12.5931721071111));
#12754=CARTESIAN_POINT('Ctrl Pts',(81.0928716977014,23.9311224971817,-12.7043052251026));
#12755=CARTESIAN_POINT('Ctrl Pts',(82.7478779500382,25.1072640883641,-12.8154383430942));
#12756=CARTESIAN_POINT('Ctrl Pts',(84.6336362259272,24.3547546447695,-12.9265714610857));
#12757=CARTESIAN_POINT('Ctrl Pts',(85.0242263285524,22.3623204276585,-13.0377045790773));
#12758=CARTESIAN_POINT('Ctrl Pts',(83.5621648225144,20.953515653978,-13.1488376970689));
#12759=CARTESIAN_POINT('Ctrl Pts',(81.5855879443197,21.4177339026156,-13.2599708150604));
#12760=CARTESIAN_POINT('Ctrl Pts',(80.903536650199,23.3301043609664,-13.371103933052));
#12761=CARTESIAN_POINT('Ctrl Pts',(82.1402511298108,24.9403503153792,-13.4822370510435));
#12762=CARTESIAN_POINT('Ctrl Pts',(84.1638416148031,24.7747112897138,-13.5933701690351));
#12763=CARTESIAN_POINT('Ctrl Pts',(85.1222384455726,22.9847866397446,-13.7045032870266));
#12764=CARTESIAN_POINT('Ctrl Pts',(84.1382791204541,21.2087858558772,-13.8156364050182));
#12765=CARTESIAN_POINT('Ctrl Pts',(82.1125219420832,21.0721747582047,-13.9267695230098));
#12766=CARTESIAN_POINT('Ctrl Pts',(80.8990196130806,22.6999852003014,-14.0379026410013));
#12767=CARTESIAN_POINT('Ctrl Pts',(81.6084172280349,24.6023809955177,-14.1490357589929));
#12768=CARTESIAN_POINT('Ctrl Pts',(83.5914461679238,25.0382146345988,-14.2601688769844));
#12769=CARTESIAN_POINT('Ctrl Pts',(85.0331602960979,23.6085940166212,-14.371301994976));
#12770=CARTESIAN_POINT('Ctrl Pts',(84.6140460963486,21.6219642008593,-14.4824351129676));
#12771=CARTESIAN_POINT('Ctrl Pts',(82.7176933820329,20.896566986924,-14.5935682309591));
#12772=CARTESIAN_POINT('Ctrl Pts',(81.0797187938726,22.0963144578846,-14.7047013489507));
#12773=CARTESIAN_POINT('Ctrl Pts',(81.1992611512568,24.123150503687,-14.8158344669422));
#12774=CARTESIAN_POINT('Ctrl Pts',(82.9669105710946,25.1220350057677,-14.9269675849338));
#12775=CARTESIAN_POINT('Ctrl Pts',(84.7648447552206,24.1787495400571,-15.0381007029254));
#12776=CARTESIAN_POINT('Ctrl Pts',(84.9475235227155,22.156626116169,-15.1492338209169));
#12777=CARTESIAN_POINT('Ctrl Pts',(83.3477521743381,20.9063916337,-15.2603669389085));
#12778=CARTESIAN_POINT('Ctrl Pts',(81.4297042171919,21.5723099953839,-15.3715000569));
#12779=CARTESIAN_POINT('Ctrl Pts',(80.9488530288205,23.5449063155938,-15.4826331748916));
#12780=CARTESIAN_POINT('Ctrl Pts',(82.3452917580788,25.0187831818178,-15.5937662928831));
#12781=CARTESIAN_POINT('Ctrl Pts',(84.340946281989,24.6449897162286,-15.7048994108747));
#12782=CARTESIAN_POINT('Ctrl Pts',(85.1093119101604,22.7656379239212,-15.8160325288663));
#12783=CARTESIAN_POINT('Ctrl Pts',(83.9471564034816,21.1007815181999,-15.9271656468578));
#12784=CARTESIAN_POINT('Ctrl Pts',(81.9181178057378,21.1741686279808,-16.0382987648494));
#12785=CARTESIAN_POINT('Ctrl Pts',(80.8792768701784,22.9186204789729,-16.149431882841));
#12786=CARTESIAN_POINT('Ctrl Pts',(81.7813723150542,24.7375700149431,-16.2605650008325));
#12787=CARTESIAN_POINT('Ctrl Pts',(83.7988693956495,24.966195283761,-16.3716981188241));
#12788=CARTESIAN_POINT('Ctrl Pts',(85.0850789011309,23.3953446611721,-16.4828312368156));
#12789=CARTESIAN_POINT('Ctrl Pts',(84.4632031240215,21.4625325565985,-16.5939643548072));
#12790=CARTESIAN_POINT('Ctrl Pts',(82.5016256568034,20.9371234393463,-16.7050974727987));
#12791=CARTESIAN_POINT('Ctrl Pts',(80.9972191663739,22.2992369991667,-16.8162305907903));
#12792=CARTESIAN_POINT('Ctrl Pts',(81.3237525783814,24.3037200750453,-16.9273637087819));
#12793=CARTESIAN_POINT('Ctrl Pts',(83.1887475863033,25.1129794781064,-17.0384968267734));
#12794=CARTESIAN_POINT('Ctrl Pts',(84.3096484764695,24.3657991545403,-17.1125855721011));
#12795=CARTESIAN_POINT('Ctrl Pts',(84.5881947811615,23.837709283723,-17.149629944765));
#12796=CARTESIAN_POINT('Ctrl Pts',(84.4664903694652,24.247266086571,-5.85037005523502));
#12797=CARTESIAN_POINT('Ctrl Pts',(84.8812182065951,23.7596440902316,-5.88741442789887));
#12798=CARTESIAN_POINT('Ctrl Pts',(85.1785105604709,22.3462470199983,-5.96150317322658));
#12799=CARTESIAN_POINT('Ctrl Pts',(83.6300855230211,20.8121128181116,-6.07263629121815));
#12800=CARTESIAN_POINT('Ctrl Pts',(81.5046932094001,21.2854931690907,-6.18376940920969));
#12801=CARTESIAN_POINT('Ctrl Pts',(80.7480335036829,23.3255834601923,-6.29490252720126));
#12802=CARTESIAN_POINT('Ctrl Pts',(82.052375241989,25.0689217816197,-6.40603564519281));
#12803=CARTESIAN_POINT('Ctrl Pts',(84.2240642092945,24.9180827510011,-6.51716876318438));
#12804=CARTESIAN_POINT('Ctrl Pts',(85.2754194831416,23.0120490775365,-6.62830188117593));
#12805=CARTESIAN_POINT('Ctrl Pts',(84.2442322933555,21.0948320889771,-6.73943499916749));
#12806=CARTESIAN_POINT('Ctrl Pts',(82.0742692171901,20.9213777396063,-6.85056811715905));
#12807=CARTESIAN_POINT('Ctrl Pts',(80.7515741571003,22.6503211972602,-6.96170123515061));
#12808=CARTESIAN_POINT('Ctrl Pts',(81.4867255381121,24.699324062942,-7.07283435314218));
#12809=CARTESIAN_POINT('Ctrl Pts',(83.6068859642405,25.1930288317273,-7.18396747113373));
#12810=CARTESIAN_POINT('Ctrl Pts',(85.1716001202748,23.6795922255951,-7.29510058912529));
#12811=CARTESIAN_POINT('Ctrl Pts',(84.748780547786,21.5441635948737,-7.40623370711685));
#12812=CARTESIAN_POINT('Ctrl Pts',(82.7254080989366,20.7411749823681,-7.51736682510841));
#12813=CARTESIAN_POINT('Ctrl Pts',(80.9533530097428,22.0055513112078,-7.62849994309997));
#12814=CARTESIAN_POINT('Ctrl Pts',(81.0544697792261,24.1800865326589,-7.73963306109152));
#12815=CARTESIAN_POINT('Ctrl Pts',(82.9362123931393,25.2745599554757,-7.85076617908309));
#12816=CARTESIAN_POINT('Ctrl Pts',(84.8763359299646,24.2872666595484,-7.96189929707464));
#12817=CARTESIAN_POINT('Ctrl Pts',(85.0991629746026,22.1218162112133,-8.0730324150662));
#12818=CARTESIAN_POINT('Ctrl Pts',(83.4007534412416,20.7601141510415,-8.18416553305776));
#12819=CARTESIAN_POINT('Ctrl Pts',(81.3355585856531,21.4484437710125,-8.29529865104933));
#12820=CARTESIAN_POINT('Ctrl Pts',(80.7937260239002,23.5568187253608,-8.40643176904088));
#12821=CARTESIAN_POINT('Ctrl Pts',(82.2711622433471,25.1555712636055,-8.51756488703244));
#12822=CARTESIAN_POINT('Ctrl Pts',(84.4156594643692,24.7814601401847,-8.628698005024));
#12823=CARTESIAN_POINT('Ctrl Pts',(85.2644894238312,22.776886578255,-8.73983112301556));
#12824=CARTESIAN_POINT('Ctrl Pts',(84.0407695331455,20.9765152018779,-8.85096424100711));
#12825=CARTESIAN_POINT('Ctrl Pts',(81.8644964014467,21.0281167561708,-8.96209735899868));
#12826=CARTESIAN_POINT('Ctrl Pts',(80.7274808561243,22.884463467863,-9.07323047699024));
#12827=CARTESIAN_POINT('Ctrl Pts',(81.6703642767617,24.8465537612011,-9.18436359498179));
#12828=CARTESIAN_POINT('Ctrl Pts',(83.8301826452576,25.11860537266,-9.29549671297336));
#12829=CARTESIAN_POINT('Ctrl Pts',(85.2301851811438,23.4516259595556,-9.40662983096491));
#12830=CARTESIAN_POINT('Ctrl Pts',(84.5890344600137,21.3713006924463,-9.51776294895647));
#12831=CARTESIAN_POINT('Ctrl Pts',(82.4935368572922,20.7816251365878,-9.62889606694804));
#12832=CARTESIAN_POINT('Ctrl Pts',(80.861574256972,22.2222935701091,-9.74002918493958));
#12833=CARTESIAN_POINT('Ctrl Pts',(81.1867830642879,24.3747495384927,-9.85116230293116));
#12834=CARTESIAN_POINT('Ctrl Pts',(83.171519378691,25.2689806196336,-9.96229542092269));
#12835=CARTESIAN_POINT('Ctrl Pts',(84.9992744067787,24.0865513314787,-10.0734285389143));
#12836=CARTESIAN_POINT('Ctrl Pts',(84.9972148071091,21.9096674985109,-10.1845616569058));
#12837=CARTESIAN_POINT('Ctrl Pts',(83.1672256063643,20.730698885975,-10.2956947748974));
#12838=CARTESIAN_POINT('Ctrl Pts',(81.1841849487392,21.6286839718163,-10.4068278928889));
#12839=CARTESIAN_POINT('Ctrl Pts',(80.863049695812,23.7817514611242,-10.5179610108805));
#12840=CARTESIAN_POINT('Ctrl Pts',(82.497735470822,25.2193292437736,-10.6290941288721));
#12841=CARTESIAN_POINT('Ctrl Pts',(84.5921135118751,24.6256895505736,-10.7402272468636));
#12842=CARTESIAN_POINT('Ctrl Pts',(85.2293266018828,22.5441547941715,-10.8513603648552));
#12843=CARTESIAN_POINT('Ctrl Pts',(83.8261722404075,20.879827512036,-10.9624934828467));
#12844=CARTESIAN_POINT('Ctrl Pts',(81.6668725266888,21.1559655400612,-11.0736266008383));
#12845=CARTESIAN_POINT('Ctrl Pts',(80.7277035479304,23.1198364863114,-11.1847597188298));
#12846=CARTESIAN_POINT('Ctrl Pts',(81.8682297188232,24.9740283635713,-11.2958928368214));
#12847=CARTESIAN_POINT('Ctrl Pts',(84.044596597093,25.0215117854914,-11.407025954813));
#12848=CARTESIAN_POINT('Ctrl Pts',(85.2649075547819,23.2188280554013,-11.5181590728046));
#12849=CARTESIAN_POINT('Ctrl Pts',(84.4122859724418,21.2158642760196,-11.6292921907961));
#12850=CARTESIAN_POINT('Ctrl Pts',(82.2670846810887,20.8458117341225,-11.7404253087877));
#12851=CARTESIAN_POINT('Ctrl Pts',(80.7926763368691,22.4473570811805,-11.8515584267792));
#12852=CARTESIAN_POINT('Ctrl Pts',(81.3384974885596,24.5547029793554,-11.9626915447708));
#12853=CARTESIAN_POINT('Ctrl Pts',(83.4049911348221,25.2391235183113,-12.0738246627623));
#12854=CARTESIAN_POINT('Ctrl Pts',(85.1008209541995,23.8742100822658,-12.1849577807539));
#12855=CARTESIAN_POINT('Ctrl Pts',(84.8738967487866,21.7091851703571,-12.2960908987455));
#12856=CARTESIAN_POINT('Ctrl Pts',(82.9319084830269,20.7255647965142,-12.407224016737));
#12857=CARTESIAN_POINT('Ctrl Pts',(81.052240253657,21.8235970417987,-12.5183571347286));
#12858=CARTESIAN_POINT('Ctrl Pts',(80.9552384072167,23.9983195771983,-12.6294902527201));
#12859=CARTESIAN_POINT('Ctrl Pts',(82.7296828515237,25.2593407420703,-12.7406233707117));
#12860=CARTESIAN_POINT('Ctrl Pts',(84.7515321896956,24.4525243330146,-12.8517564887033));
#12861=CARTESIAN_POINT('Ctrl Pts',(85.1703103282228,22.3163004835832,-12.9628896066948));
#12862=CARTESIAN_POINT('Ctrl Pts',(83.6027350317784,20.8058253417273,-13.0740227246864));
#12863=CARTESIAN_POINT('Ctrl Pts',(81.4835129108309,21.3035452089955,-13.1851558426779));
#12864=CARTESIAN_POINT('Ctrl Pts',(80.7522394622406,23.3539272728011,-13.2962889606695));
#12865=CARTESIAN_POINT('Ctrl Pts',(82.0782049288016,25.080381166097,-13.407422078661));
#12866=CARTESIAN_POINT('Ctrl Pts',(84.2478335260214,24.9027883331771,-13.5185551966526));
#12867=CARTESIAN_POINT('Ctrl Pts',(85.2753957659822,22.9836887247125,-13.6296883146442));
#12868=CARTESIAN_POINT('Ctrl Pts',(84.2204262422021,21.0795178374008,-13.7408214326357));
#12869=CARTESIAN_POINT('Ctrl Pts',(82.0484745860681,20.9330478147326,-13.8519545506273));
#12870=CARTESIAN_POINT('Ctrl Pts',(80.7473964404041,22.6783337864837,-13.9630876686188));
#12871=CARTESIAN_POINT('Ctrl Pts',(81.5079897341654,24.7180213374692,-14.0742207866104));
#12872=CARTESIAN_POINT('Ctrl Pts',(83.6341295480289,25.1853081398107,-14.185353904602));
#12873=CARTESIAN_POINT('Ctrl Pts',(85.1798890407227,23.6525149195704,-14.2964870225935));
#12874=CARTESIAN_POINT('Ctrl Pts',(84.7305282831878,21.5225143624751,-14.4076201405851));
#12875=CARTESIAN_POINT('Ctrl Pts',(82.6973199290724,20.7447668135665,-14.5187532585766));
#12876=CARTESIAN_POINT('Ctrl Pts',(80.9411362870026,22.0310974430802,-14.6298863765682));
#12877=CARTESIAN_POINT('Ctrl Pts',(81.0693057556195,24.2042058261558,-14.7410194945597));
#12878=CARTESIAN_POINT('Ctrl Pts',(82.9645225791725,25.2751776443702,-14.8521526125513));
#12879=CARTESIAN_POINT('Ctrl Pts',(84.8922097524064,24.2638173237295,-14.9632857305429));
#12880=CARTESIAN_POINT('Ctrl Pts',(85.0880720481635,22.0957616622145,-15.0744188485344));
#12881=CARTESIAN_POINT('Ctrl Pts',(83.372848690377,20.7553004836746,-15.185551966526));
#12882=CARTESIAN_POINT('Ctrl Pts',(81.3163793950698,21.4692767212771,-15.2966850845175));
#12883=CARTESIAN_POINT('Ctrl Pts',(80.8008262250806,23.5842310160509,-15.4078182025091));
#12884=CARTESIAN_POINT('Ctrl Pts',(82.2980428920563,25.1644743614589,-15.5189513205007));
#12885=CARTESIAN_POINT('Ctrl Pts',(84.4377194508057,24.7637050366322,-15.6300844384922));
#12886=CARTESIAN_POINT('Ctrl Pts',(85.2615363506997,22.7487245239907,-15.7412175564838));
#12887=CARTESIAN_POINT('Ctrl Pts',(84.0155106155488,20.9637190622108,-15.8523506744753));
#12888=CARTESIAN_POINT('Ctrl Pts',(81.8400407271619,21.0424023596608,-15.9634837924669));
#12889=CARTESIAN_POINT('Ctrl Pts',(80.7262289068018,22.9127474964141,-16.0746169104585));
#12890=CARTESIAN_POINT('Ctrl Pts',(81.6934266126323,24.8629666536045,-16.18575002845));
#12891=CARTESIAN_POINT('Ctrl Pts',(83.8565220577477,25.1080913094838,-16.2968831464416));
#12892=CARTESIAN_POINT('Ctrl Pts',(85.2355544982563,23.4238758231957,-16.4080162644331));
#12893=CARTESIAN_POINT('Ctrl Pts',(84.5687993025081,21.3515768841388,-16.5191493824247));
#12894=CARTESIAN_POINT('Ctrl Pts',(82.4656590673167,20.7882501367141,-16.6302825004163));
#12895=CARTESIAN_POINT('Ctrl Pts',(80.8526828413037,22.2486644616303,-16.7414156184078));
#12896=CARTESIAN_POINT('Ctrl Pts',(81.2027814575469,24.3978067096903,-16.8525487363994));
#12897=CARTESIAN_POINT('Ctrl Pts',(83.2023690879836,25.2654685990261,-16.9636818543909));
#12898=CARTESIAN_POINT('Ctrl Pts',(84.4041629509165,24.4643659009695,-17.0377705997186));
#12899=CARTESIAN_POINT('Ctrl Pts',(84.7028113349605,23.8981649358411,-17.0748149723825));
#12900=CARTESIAN_POINT('Ctrl Pts',(84.5652001142717,24.3312198033322,-5.77555508285253));
#12901=CARTESIAN_POINT('Ctrl Pts',(85.0078433607487,23.8107758779691,-5.81259945551639));
#12902=CARTESIAN_POINT('Ctrl Pts',(85.3251465193287,22.3022427829668,-5.88668820084409));
#12903=CARTESIAN_POINT('Ctrl Pts',(83.6724966990361,20.6648457170885,-5.99782131883566));
#12904=CARTESIAN_POINT('Ctrl Pts',(81.4040438258236,21.170089389242,-6.1089544368272));
#12905=CARTESIAN_POINT('Ctrl Pts',(80.5964532118565,23.3474985446265,-6.22008755481878));
#12906=CARTESIAN_POINT('Ctrl Pts',(81.9885904398633,25.2081812989956,-6.33122067281032));
#12907=CARTESIAN_POINT('Ctrl Pts',(84.3064562032972,25.0471892646279,-6.44235379080189));
#12908=CARTESIAN_POINT('Ctrl Pts',(85.4285783999577,23.0128601032299,-6.55348690879345));
#12909=CARTESIAN_POINT('Ctrl Pts',(84.3279818049202,20.9665948756778,-6.664620026785));
#12910=CARTESIAN_POINT('Ctrl Pts',(82.0119581026862,20.781465281165,-6.77575314477657));
#12911=CARTESIAN_POINT('Ctrl Pts',(80.6002321873268,22.6267842507508,-6.88688626276812));
#12912=CARTESIAN_POINT('Ctrl Pts',(81.3848667471746,24.8137058878003,-6.99801938075968));
#12913=CARTESIAN_POINT('Ctrl Pts',(83.6477355735556,25.340642018176,-7.10915249875124));
#12914=CARTESIAN_POINT('Ctrl Pts',(85.3177709360927,23.7253357071464,-7.2202856167428));
#12915=CARTESIAN_POINT('Ctrl Pts',(84.8664912980158,21.4461709704268,-7.33141873473436));
#12916=CARTESIAN_POINT('Ctrl Pts',(82.706925266015,20.5891330421716,-7.44255185272592));
#12917=CARTESIAN_POINT('Ctrl Pts',(80.8155928127967,21.9386147814237,-7.55368497071748));
#12918=CARTESIAN_POINT('Ctrl Pts',(80.923515771205,24.2595183809094,-7.66481808870904));
#12919=CARTESIAN_POINT('Ctrl Pts',(82.9319188372278,25.4276610173216,-7.7759512067006));
#12920=CARTESIAN_POINT('Ctrl Pts',(85.0026324571524,24.3739128224606,-7.88708432469215));
#12921=CARTESIAN_POINT('Ctrl Pts',(85.2404580324118,22.0627054938917,-7.99821744268371));
#12922=CARTESIAN_POINT('Ctrl Pts',(83.427728231352,20.6093470098792,-8.10935056067528));
#12923=CARTESIAN_POINT('Ctrl Pts',(81.2235247184853,21.3440082270736,-8.22048367866683));
#12924=CARTESIAN_POINT('Ctrl Pts',(80.6452213042727,23.5942982993343,-8.33161679665839));
#12925=CARTESIAN_POINT('Ctrl Pts',(82.2221040357635,25.3006631740422,-8.44274991464995));
#12926=CARTESIAN_POINT('Ctrl Pts',(84.5109477713164,24.9013705599747,-8.55388303264151));
#12927=CARTESIAN_POINT('Ctrl Pts',(85.4169126362828,22.7618687715364,-8.66501615063307));
#12928=CARTESIAN_POINT('Ctrl Pts',(84.1108239277452,20.8403140564757,-8.77614926862462));
#12929=CARTESIAN_POINT('Ctrl Pts',(81.7880654389434,20.8953889211715,-8.88728238661619));
#12930=CARTESIAN_POINT('Ctrl Pts',(80.574517161694,22.8766866819798,-8.99841550460775));
#12931=CARTESIAN_POINT('Ctrl Pts',(81.5808662441396,24.9708456449631,-9.10954862259931));
#12932=CARTESIAN_POINT('Ctrl Pts',(83.8860623965075,25.2612091019686,-9.22068174059087));
#12933=CARTESIAN_POINT('Ctrl Pts',(85.3802993685163,23.4820249885188,-9.33181485858242));
#12934=CARTESIAN_POINT('Ctrl Pts',(84.6959926707885,21.2616726332633,-9.44294797657398));
#12935=CARTESIAN_POINT('Ctrl Pts',(82.4594467271343,20.632305903941,-9.55408109456555));
#12936=CARTESIAN_POINT('Ctrl Pts',(80.7176364147761,22.1699460028647,-9.66521421255709));
#12937=CARTESIAN_POINT('Ctrl Pts',(81.0647350885701,24.4672841905729,-9.77634733054866));
#12938=CARTESIAN_POINT('Ctrl Pts',(83.1830643805896,25.4217061353262,-9.88748044854022));
#12939=CARTESIAN_POINT('Ctrl Pts',(85.1338459461496,24.1596873076041,-9.99861356653177));
#12940=CARTESIAN_POINT('Ctrl Pts',(85.1316477144354,21.8362770111152,-10.1097466845233));
#12941=CARTESIAN_POINT('Ctrl Pts',(83.1784815936336,20.5779517977441,-10.2208798025149));
#12942=CARTESIAN_POINT('Ctrl Pts',(81.0619620933712,21.536380429966,-10.3320129205065));
#12943=CARTESIAN_POINT('Ctrl Pts',(80.7192111656842,23.8343713001878,-10.443146038498));
#12944=CARTESIAN_POINT('Ctrl Pts',(82.4639279501368,25.3687127159435,-10.5542791564896));
#12945=CARTESIAN_POINT('Ctrl Pts',(84.6992789742144,24.7351150224436,-10.6654122744811));
#12946=CARTESIAN_POINT('Ctrl Pts',(85.3793829981224,22.5134717669416,-10.7765453924727));
#12947=CARTESIAN_POINT('Ctrl Pts',(83.8817820505465,20.7371182998993,-10.8876785104642));
#12948=CARTESIAN_POINT('Ctrl Pts',(81.5771394637072,21.0318432309449,-10.9988116284558));
#12949=CARTESIAN_POINT('Ctrl Pts',(80.574754842928,23.1279027029253,-11.1099447464474));
#12950=CARTESIAN_POINT('Ctrl Pts',(81.7920500466204,25.1069005869871,-11.2210778644389));
#12951=CARTESIAN_POINT('Ctrl Pts',(84.1149085920925,25.1575801270393,-11.3322109824305));
#12952=CARTESIAN_POINT('Ctrl Pts',(85.4173589117072,23.2335574132988,-11.4433441004221));
#12953=CARTESIAN_POINT('Ctrl Pts',(84.5073472090078,21.0957737621771,-11.5544772184136));
#12954=CARTESIAN_POINT('Ctrl Pts',(82.2177520120164,20.7008129135252,-11.6656103364052));
#12955=CARTESIAN_POINT('Ctrl Pts',(80.6441009626085,22.410158581537,-11.7767434543967));
#12956=CARTESIAN_POINT('Ctrl Pts',(81.2266614395036,24.6593503316581,-11.8878765723883));
#12957=CARTESIAN_POINT('Ctrl Pts',(83.4322511648908,25.3898393468531,-11.9990096903799));
#12958=CARTESIAN_POINT('Ctrl Pts',(85.2422276109297,23.9330533286481,-12.1101428083714));
#12959=CARTESIAN_POINT('Ctrl Pts',(85.000029094227,21.6223001794432,-12.221275926363));
#12960=CARTESIAN_POINT('Ctrl Pts',(82.9273252301097,20.5724721317484,-12.3324090443545));
#12961=CARTESIAN_POINT('Ctrl Pts',(80.9211361758472,21.7444131356433,-12.4435421623461));
#12962=CARTESIAN_POINT('Ctrl Pts',(80.8176051167319,24.0655166572149,-12.5546752803376));
#12963=CARTESIAN_POINT('Ctrl Pts',(82.7114877530095,25.4114173957764,-12.6658083983292));
#12964=CARTESIAN_POINT('Ctrl Pts',(84.8694281534639,24.5502940212596,-12.7769415163208));
#12965=CARTESIAN_POINT('Ctrl Pts',(85.3163943278932,22.2702805395079,-12.8880746343123));
#12966=CARTESIAN_POINT('Ctrl Pts',(83.6433052410424,20.6581350294767,-12.9992077523039));
#12967=CARTESIAN_POINT('Ctrl Pts',(81.381437877342,21.1893565153754,-13.1103408702954));
#12968=CARTESIAN_POINT('Ctrl Pts',(80.6009422742822,23.3777501846358,-13.221473988287));
#12969=CARTESIAN_POINT('Ctrl Pts',(82.0161587277924,25.2204120168147,-13.3326071062785));
#12970=CARTESIAN_POINT('Ctrl Pts',(84.3318254372397,25.0308653766405,-13.4437402242701));
#12971=CARTESIAN_POINT('Ctrl Pts',(85.4285530863916,22.9825908096803,-13.5548733422617));
#12972=CARTESIAN_POINT('Ctrl Pts',(84.3025733639503,20.9502498189244,-13.6660064602532));
#12973=CARTESIAN_POINT('Ctrl Pts',(81.9844272300528,20.7939208712606,-13.7771395782448));
#12974=CARTESIAN_POINT('Ctrl Pts',(80.5957732677276,22.6566823726659,-13.8882726962363));
#12975=CARTESIAN_POINT('Ctrl Pts',(81.407562240296,24.8336616794208,-13.9994058142279));
#12976=CARTESIAN_POINT('Ctrl Pts',(83.6768129281338,25.3324016450226,-14.1105389322195));
#12977=CARTESIAN_POINT('Ctrl Pts',(85.3266177853476,23.6964358225195,-14.221672050211));
#12978=CARTESIAN_POINT('Ctrl Pts',(84.8470104700268,21.423064524091,-14.3328051682026));
#12979=CARTESIAN_POINT('Ctrl Pts',(82.676946476112,20.5929666402091,-14.4439382861941));
#12980=CARTESIAN_POINT('Ctrl Pts',(80.8025537801326,21.9658804282759,-14.5550714041857));
#12981=CARTESIAN_POINT('Ctrl Pts',(80.9393503599823,24.2852611486245,-14.6662045221773));
#12982=CARTESIAN_POINT('Ctrl Pts',(82.9621345872503,25.4283202829728,-14.7773376401688));
#12983=CARTESIAN_POINT('Ctrl Pts',(85.0195747495924,24.3488851074018,-14.8884707581604));
#12984=CARTESIAN_POINT('Ctrl Pts',(85.2286205736113,22.0348972082601,-14.9996038761519));
#12985=CARTESIAN_POINT('Ctrl Pts',(83.3979452064162,20.6042093336492,-15.1107369941435));
#12986=CARTESIAN_POINT('Ctrl Pts',(81.2030545729478,21.3662434471704,-15.221870112135));
#12987=CARTESIAN_POINT('Ctrl Pts',(80.6527994213405,23.6235557165079,-15.3330032301266));
#12988=CARTESIAN_POINT('Ctrl Pts',(82.2507940260338,25.3101655411,-15.4441363481181));
#12989=CARTESIAN_POINT('Ctrl Pts',(84.5344926196224,24.8824203570357,-15.5552694661097));
#12990=CARTESIAN_POINT('Ctrl Pts',(85.4137607912389,22.7318111240602,-15.6664025841013));
#12991=CARTESIAN_POINT('Ctrl Pts',(84.0838648276161,20.8266566062216,-15.7775357020929));
#12992=CARTESIAN_POINT('Ctrl Pts',(81.7619636485858,20.9106360913409,-15.8886688200844));
#12993=CARTESIAN_POINT('Ctrl Pts',(80.5731809434253,22.9068745138551,-15.999801938076));
#12994=CARTESIAN_POINT('Ctrl Pts',(81.60548091021,24.9883632922658,-16.1109350560675));
#12995=CARTESIAN_POINT('Ctrl Pts',(83.9141747198462,25.2499873352066,-16.2220681740591));
#12996=CARTESIAN_POINT('Ctrl Pts',(85.3860300953815,23.4524069852193,-16.3332012920506));
#12997=CARTESIAN_POINT('Ctrl Pts',(84.6743954809949,21.240621211679,-16.4443344100422));
#12998=CARTESIAN_POINT('Ctrl Pts',(82.4296924778299,20.6393768340819,-16.5554675280338));
#12999=CARTESIAN_POINT('Ctrl Pts',(80.7081465162334,22.1980919240939,-16.6666006460253));
#13000=CARTESIAN_POINT('Ctrl Pts',(81.0818103367127,24.4918933443353,-16.7777337640169));
#13001=CARTESIAN_POINT('Ctrl Pts',(83.2159905896636,25.4179577199457,-16.8888668820084));
#13002=CARTESIAN_POINT('Ctrl Pts',(84.4986774253636,24.5629326473987,-16.9629556273361));
#13003=CARTESIAN_POINT('Ctrl Pts',(84.8174278887595,23.9586205879593,-17.));
#13004=CARTESIAN_POINT('Ctrl Pts',(84.2690708798524,24.0793586530485,-6.));
#13005=CARTESIAN_POINT('Ctrl Pts',(84.31440001981,24.0370713763938,-6.));
#13006=CARTESIAN_POINT('Ctrl Pts',(84.3569991508135,23.9922149796692,-6.));
#13007=CARTESIAN_POINT('Ctrl Pts',(84.3968697551056,23.9451344884964,-6.));
#13008=CARTESIAN_POINT('Ctrl Pts',(84.4393720233826,23.8949464438965,-6.));
#13009=CARTESIAN_POINT('Ctrl Pts',(84.478774408848,23.8422307785529,-6.));
#13010=CARTESIAN_POINT('Ctrl Pts',(84.5150498742739,23.7873507314227,-6.));
#13011=CARTESIAN_POINT('Ctrl Pts',(84.5467909065216,23.7393306901838,-6.));
#13012=CARTESIAN_POINT('Ctrl Pts',(84.5761376471904,23.6896523185269,-6.));
#13013=CARTESIAN_POINT('Ctrl Pts',(84.6030490903269,23.6385314038462,-6.));
#13014=CARTESIAN_POINT('Ctrl Pts',(84.6165493141079,23.6128864102062,-6.));
#13015=CARTESIAN_POINT('Ctrl Pts',(84.6294363190557,23.5868780356607,-6.));
#13016=CARTESIAN_POINT('Ctrl Pts',(84.6417025870925,23.5605316810879,-6.));
#13017=CARTESIAN_POINT('Ctrl Pts',(84.647311574959,23.5484843018295,-6.));
#13018=CARTESIAN_POINT('Ctrl Pts',(84.652791347877,23.5363645681783,-6.));
#13019=CARTESIAN_POINT('Ctrl Pts',(84.6581326742843,23.5241948681676,-6.));
#13020=CARTESIAN_POINT('Ctrl Pts',(84.6850515361933,23.4628628227009,-6.));
#13021=CARTESIAN_POINT('Ctrl Pts',(84.7085092386931,23.400155314048,-6.));
#13022=CARTESIAN_POINT('Ctrl Pts',(84.7284822796849,23.3364301112262,-6.));
#13023=CARTESIAN_POINT('Ctrl Pts',(84.7488096464292,23.2715744105277,-6.));
#13024=CARTESIAN_POINT('Ctrl Pts',(84.7655281752392,23.2056637457477,-6.));
#13025=CARTESIAN_POINT('Ctrl Pts',(84.7785737746937,23.139038753957,-6.));
#13026=CARTESIAN_POINT('Ctrl Pts',(84.7894849804243,23.083314293401,-6.));
#13027=CARTESIAN_POINT('Ctrl Pts',(84.7978262414115,23.0270891857862,-6.));
#13028=CARTESIAN_POINT('Ctrl Pts',(84.8035352337538,22.9705504503036,-6.));
#13029=CARTESIAN_POINT('Ctrl Pts',(84.8061648366007,22.9445083029563,-6.));
#13030=CARTESIAN_POINT('Ctrl Pts',(84.8082356449419,22.9183995035543,-6.));
#13031=CARTESIAN_POINT('Ctrl Pts',(84.8097397666649,22.8922419268446,-6.));
#13032=CARTESIAN_POINT('Ctrl Pts',(84.8103971308092,22.8808099710605,-6.));
#13033=CARTESIAN_POINT('Ctrl Pts',(84.8109461375351,22.8693689032805,-6.));
#13034=CARTESIAN_POINT('Ctrl Pts',(84.8113857933626,22.8579343510023,-6.));
#13035=CARTESIAN_POINT('Ctrl Pts',(84.8140821318782,22.7878080799712,-6.));
#13036=CARTESIAN_POINT('Ctrl Pts',(84.8126777401308,22.7177955074969,-6.));
#13037=CARTESIAN_POINT('Ctrl Pts',(84.8071179912164,22.6482574382939,-6.));
#13038=CARTESIAN_POINT('Ctrl Pts',(84.8021484095824,22.5861008342993,-6.));
#13039=CARTESIAN_POINT('Ctrl Pts',(84.7938584808496,22.5243223796457,-6.));
#13040=CARTESIAN_POINT('Ctrl Pts',(84.7821760832888,22.4631676164083,-6.));
#13041=CARTESIAN_POINT('Ctrl Pts',(84.7694456203586,22.3965264631396,-6.));
#13042=CARTESIAN_POINT('Ctrl Pts',(84.7526877740569,22.3306250945486,-6.));
#13043=CARTESIAN_POINT('Ctrl Pts',(84.7321477736998,22.2656770857153,-6.));
#13044=CARTESIAN_POINT('Ctrl Pts',(84.7242184256731,22.2406042835379,-6.));
#13045=CARTESIAN_POINT('Ctrl Pts',(84.7157248685372,22.2156736078728,-6.));
#13046=CARTESIAN_POINT('Ctrl Pts',(84.7066792009377,22.1908976666699,-6.));
#13047=CARTESIAN_POINT('Ctrl Pts',(84.702711832254,22.1800311062797,-6.));
#13048=CARTESIAN_POINT('Ctrl Pts',(84.6986383589894,22.1691948787475,-6.));
#13049=CARTESIAN_POINT('Ctrl Pts',(84.6944648872271,22.158402584267,-6.));
#13050=CARTESIAN_POINT('Ctrl Pts',(84.6692420795077,22.093178237719,-6.));
#13051=CARTESIAN_POINT('Ctrl Pts',(84.6403284563561,22.0294393145623,-6.));
#13052=CARTESIAN_POINT('Ctrl Pts',(84.6080366728143,21.9674046173891,-6.));
#13053=CARTESIAN_POINT('Ctrl Pts',(84.5749968927465,21.9039329683697,-6.));
#13054=CARTESIAN_POINT('Ctrl Pts',(84.5384203362702,21.8422445927193,-6.));
#13055=CARTESIAN_POINT('Ctrl Pts',(84.4985857546133,21.7825775666462,-6.));
#13056=CARTESIAN_POINT('Ctrl Pts',(84.4680931898081,21.736903667647,-6.));
#13057=CARTESIAN_POINT('Ctrl Pts',(84.4356903395602,21.6924141647768,-6.));
#13058=CARTESIAN_POINT('Ctrl Pts',(84.4014826868376,21.6492219482087,-6.));
#13059=CARTESIAN_POINT('Ctrl Pts',(84.3801861847344,21.6223319672315,-6.));
#13060=CARTESIAN_POINT('Ctrl Pts',(84.3581898396724,21.5959449213339,-6.));
#13061=CARTESIAN_POINT('Ctrl Pts',(84.3355161968359,21.5700897403578,-6.));
#13062=CARTESIAN_POINT('Ctrl Pts',(84.3228380888485,21.5556326555914,-6.));
#13063=CARTESIAN_POINT('Ctrl Pts',(84.3099437537492,21.5413373293104,-6.));
#13064=CARTESIAN_POINT('Ctrl Pts',(84.2968608165032,21.5272342242042,-6.));
#13065=CARTESIAN_POINT('Ctrl Pts',(84.2459896381448,21.4723962652833,-6.));
#13066=CARTESIAN_POINT('Ctrl Pts',(84.1922219184366,21.4204032503112,-6.));
#13067=CARTESIAN_POINT('Ctrl Pts',(84.1358426011268,21.3715190959182,-6.));
#13068=CARTESIAN_POINT('Ctrl Pts',(84.0936830787195,21.3349643325611,-6.));
#13069=CARTESIAN_POINT('Ctrl Pts',(84.0500620462463,21.3001481807965,-6.));
#13070=CARTESIAN_POINT('Ctrl Pts',(84.0050822634579,21.2671907406919,-6.));
#13071=CARTESIAN_POINT('Ctrl Pts',(83.9910186215557,21.2568860747528,-6.));
#13072=CARTESIAN_POINT('Ctrl Pts',(83.9768220557377,21.2467631932491,-6.));
#13073=CARTESIAN_POINT('Ctrl Pts',(83.9624954655677,21.2368259940225,-6.));
#13074=CARTESIAN_POINT('Ctrl Pts',(83.9487061337562,21.2272614475543,-6.));
#13075=CARTESIAN_POINT('Ctrl Pts',(83.9348033877552,21.2178738647995,-6.));
#13076=CARTESIAN_POINT('Ctrl Pts',(83.9207951867164,21.2086694621281,-6.));
#13077=CARTESIAN_POINT('Ctrl Pts',(83.8578415491727,21.1673043626424,-6.));
#13078=CARTESIAN_POINT('Ctrl Pts',(83.7927304527034,21.1296149339887,-6.));
#13079=CARTESIAN_POINT('Ctrl Pts',(83.7257231789248,21.0958803410021,-6.));
#13080=CARTESIAN_POINT('Ctrl Pts',(83.6744958173968,21.0700900932652,-6.));
#13081=CARTESIAN_POINT('Ctrl Pts',(83.6221592285687,21.0466117245125,-6.));
#13082=CARTESIAN_POINT('Ctrl Pts',(83.5688162931808,21.0255852276549,-6.));
#13083=CARTESIAN_POINT('Ctrl Pts',(83.5563690536895,21.0206788264576,-6.));
#13084=CARTESIAN_POINT('Ctrl Pts',(83.5438669750959,21.0159059951676,-6.));
#13085=CARTESIAN_POINT('Ctrl Pts',(83.5313119958266,21.0112661450614,-6.));
#13086=CARTESIAN_POINT('Ctrl Pts',(81.3326822579993,22.9986976815004,-7.12851963660979));
#13087=CARTESIAN_POINT('Ctrl Pts',(81.3319479721743,22.9132137610073,-7.12279015104506));
#13088=CARTESIAN_POINT('Ctrl Pts',(81.3379545916533,22.8278333679087,-7.11706066548032));
#13089=CARTESIAN_POINT('Ctrl Pts',(81.3510611587958,22.7435572384718,-7.11133117991559));
#13090=CARTESIAN_POINT('Ctrl Pts',(81.4358025464977,22.1986642790157,-7.07428680725174));
#13091=CARTESIAN_POINT('Ctrl Pts',(81.8173469963478,21.6999334677524,-7.03724243458788));
#13092=CARTESIAN_POINT('Ctrl Pts',(82.3210928586109,21.4755853719685,-7.00019806192403));
#13093=CARTESIAN_POINT('Ctrl Pts',(82.824838720874,21.2512372761846,-6.96315368926018));
#13094=CARTESIAN_POINT('Ctrl Pts',(83.45078599555,21.3012718958802,-6.92610931659632));
#13095=CARTESIAN_POINT('Ctrl Pts',(83.9124876961019,21.6028092908236,-6.88906494393247));
#13096=CARTESIAN_POINT('Ctrl Pts',(84.3741893966538,21.904346685767,-6.85202057126862));
#13097=CARTESIAN_POINT('Ctrl Pts',(84.6716455230816,22.4573868559583,-6.81497619860477));
#13098=CARTESIAN_POINT('Ctrl Pts',(84.6687366815921,23.0088140573203,-6.77793182594091));
#13099=CARTESIAN_POINT('Ctrl Pts',(84.6658278401026,23.5602412586823,-6.74088745327706));
#13100=CARTESIAN_POINT('Ctrl Pts',(84.3625540306957,24.1100554912149,-6.70384308061321));
#13101=CARTESIAN_POINT('Ctrl Pts',(83.8976945634842,24.4067181113346,-6.66679870794935));
#13102=CARTESIAN_POINT('Ctrl Pts',(83.4328350962727,24.7033807314542,-6.6297543352855));
#13103=CARTESIAN_POINT('Ctrl Pts',(82.8063899712565,24.746891739161,-6.59270996262165));
#13104=CARTESIAN_POINT('Ctrl Pts',(82.3050422822643,24.5172056670904,-6.5556655899578));
#13105=CARTESIAN_POINT('Ctrl Pts',(81.8036945932721,24.2875195950198,-6.51862121729394));
#13106=CARTESIAN_POINT('Ctrl Pts',(81.4274443403038,23.7846364431718,-6.48157684463009));
#13107=CARTESIAN_POINT('Ctrl Pts',(81.3484521953559,23.2389527734919,-6.44453247196624));
#13108=CARTESIAN_POINT('Ctrl Pts',(81.3370704557417,23.1603268614577,-6.43919486018075));
#13109=CARTESIAN_POINT('Ctrl Pts',(81.3318601088966,23.080812365398,-6.43385724839527));
#13110=CARTESIAN_POINT('Ctrl Pts',(81.3325224760112,23.0012132743929,-6.42851963660979));
#13111=CARTESIAN_POINT('Ctrl Pts',(82.4698297828114,21.0148256743283,-6.));
#13112=CARTESIAN_POINT('Ctrl Pts',(81.8097404375819,21.1911123142463,-6.03704437266385));
#13113=CARTESIAN_POINT('Ctrl Pts',(80.6907279345985,22.2513783981503,-6.11113311799155));
#13114=CARTESIAN_POINT('Ctrl Pts',(81.1186741999742,24.5381192006252,-6.22226623598312));
#13115=CARTESIAN_POINT('Ctrl Pts',(83.2718171861771,25.4128332182024,-6.33339935397467));
#13116=CARTESIAN_POINT('Ctrl Pts',(85.1745320403748,24.0812968093214,-6.44453247196624));
#13117=CARTESIAN_POINT('Ctrl Pts',(85.0878555272437,21.7590837146758,-6.55566558995779));
#13118=CARTESIAN_POINT('Ctrl Pts',(83.0898774457969,20.5731226537472,-6.66679870794935));
#13119=CARTESIAN_POINT('Ctrl Pts',(81.0098475676149,21.6080762686228,-6.77793182594092));
#13120=CARTESIAN_POINT('Ctrl Pts',(80.7511794463617,23.9171031255975,-6.88906494393247));
#13121=CARTESIAN_POINT('Ctrl Pts',(82.5507725952567,25.3866959940047,-7.00019806192404));
#13122=CARTESIAN_POINT('Ctrl Pts',(84.7614901796242,24.6719233964163,-7.11133117991558));
#13123=CARTESIAN_POINT('Ctrl Pts',(85.3600357402078,22.4269243306697,-7.22246429790715));
#13124=CARTESIAN_POINT('Ctrl Pts',(83.7985771227055,20.7064348813032,-7.33359741589871));
#13125=CARTESIAN_POINT('Ctrl Pts',(81.5062325893395,21.0851023869821,-7.44473053389026));
#13126=CARTESIAN_POINT('Ctrl Pts',(80.5810411304203,23.2163616212335,-7.55586365188184));
#13127=CARTESIAN_POINT('Ctrl Pts',(81.8697768675109,25.1495971491679,-7.66699676987337));
#13128=CARTESIAN_POINT('Ctrl Pts',(84.1929368847996,25.1154372776465,-7.77812988786495));
#13129=CARTESIAN_POINT('Ctrl Pts',(85.4242743200689,23.1451456867025,-7.8892630058565));
#13130=CARTESIAN_POINT('Ctrl Pts',(84.4368203745666,21.042011180836,-8.00039612384806));
#13131=CARTESIAN_POINT('Ctrl Pts',(82.1343319219779,20.7309050425608,-8.11152924183962));
#13132=CARTESIAN_POINT('Ctrl Pts',(80.6241369404767,22.4965639528314,-8.22266235983118));
#13133=CARTESIAN_POINT('Ctrl Pts',(81.2884253572881,24.7229873320792,-8.33379547782273));
#13134=CARTESIAN_POINT('Ctrl Pts',(83.5192142474232,25.3724648971313,-8.44492859581431));
#13135=CARTESIAN_POINT('Ctrl Pts',(85.2747978255561,23.850569204887,-8.55606171380586));
#13136=CARTESIAN_POINT('Ctrl Pts',(84.9483968969088,21.5501991003249,-8.66719483179741));
#13137=CARTESIAN_POINT('Ctrl Pts',(82.8387464408891,20.5767438417137,-8.77832794978898));
#13138=CARTESIAN_POINT('Ctrl Pts',(80.8766815886281,21.8211479981201,-8.88946106778053));
#13139=CARTESIAN_POINT('Ctrl Pts',(80.8579613196625,24.1444839055483,-9.00059418577209));
#13140=CARTESIAN_POINT('Ctrl Pts',(82.7997191606577,25.4203430963022,-9.11172730376366));
#13141=CARTESIAN_POINT('Ctrl Pts',(84.9247819088485,24.4810090214786,-9.22286042175521));
#13142=CARTESIAN_POINT('Ctrl Pts',(85.2882084953573,22.1861971982837,-9.33399353974677));
#13143=CARTESIAN_POINT('Ctrl Pts',(83.5573766039194,20.6362097301691,-9.44512665773833));
#13144=CARTESIAN_POINT('Ctrl Pts',(81.3164117064387,21.2496561548905,-9.55625977572989));
#13145=CARTESIAN_POINT('Ctrl Pts',(80.6163330806179,23.4650861595143,-9.66739289372146));
#13146=CARTESIAN_POINT('Ctrl Pts',(82.0978802396299,25.2548510053398,-9.778526011713));
#13147=CARTESIAN_POINT('Ctrl Pts',(84.4050829104209,24.9808874610066,-9.88965912970457));
#13148=CARTESIAN_POINT('Ctrl Pts',(85.4262983980702,22.8939377453899,-10.0007922476961));
#13149=CARTESIAN_POINT('Ctrl Pts',(84.2268700936312,20.9040603797618,-10.1119253656877));
#13150=CARTESIAN_POINT('Ctrl Pts',(81.9045619903646,20.8324694499553,-10.2230584836792));
#13151=CARTESIAN_POINT('Ctrl Pts',(80.5848418695363,22.7446877927209,-10.3341916016708));
#13152=CARTESIAN_POINT('Ctrl Pts',(81.4755695294061,24.8905779165788,-10.4453247196624));
#13153=CARTESIAN_POINT('Ctrl Pts',(83.7615159569619,25.3061367187622,-10.5564578376539));
#13154=CARTESIAN_POINT('Ctrl Pts',(85.3504930077305,23.6110284272776,-10.6675909556455));
#13155=CARTESIAN_POINT('Ctrl Pts',(84.7882063433206,21.3566828693041,-10.778724073637));
#13156=CARTESIAN_POINT('Ctrl Pts',(82.5892828503881,20.6063658296754,-10.8898571916286));
#13157=CARTESIAN_POINT('Ctrl Pts',(80.7662638584498,22.0467969952507,-11.0009903096202));
#13158=CARTESIAN_POINT('Ctrl Pts',(80.987648102256,24.3596370684772,-11.1121234276117));
#13159=CARTESIAN_POINT('Ctrl Pts',(83.0508160082765,25.4280837818398,-11.2232565456033));
#13160=CARTESIAN_POINT('Ctrl Pts',(85.0674751034236,24.2742526496163,-11.3343896635948));
#13161=CARTESIAN_POINT('Ctrl Pts',(85.1918996088904,21.9541753383684,-11.4455227815864));
#13162=CARTESIAN_POINT('Ctrl Pts',(83.3102113199728,20.5912779207033,-11.5566558995779));
#13163=CARTESIAN_POINT('Ctrl Pts',(81.1446054212175,21.4329377563877,-11.6677890175695));
#13164=CARTESIAN_POINT('Ctrl Pts',(80.6771296685829,23.708834636395,-11.7789221355611));
#13165=CARTESIAN_POINT('Ctrl Pts',(82.3356362705467,25.3359781577142,-11.8900552535526));
#13166=CARTESIAN_POINT('Ctrl Pts',(84.6021947068076,24.825142525889,-12.0011883715442));
#13167=CARTESIAN_POINT('Ctrl Pts',(85.4023614856292,22.6438646174604,-12.1123214895358));
#13168=CARTESIAN_POINT('Ctrl Pts',(84.0037924767762,20.7885358284841,-12.2234546075273));
#13169=CARTESIAN_POINT('Ctrl Pts',(81.6865130842908,20.9572260916608,-12.3345877255189));
#13170=CARTESIAN_POINT('Ctrl Pts',(80.5713886154037,22.995543438547,-12.4457208435104));
#13171=CARTESIAN_POINT('Ctrl Pts',(81.6790248749117,25.0379396058836,-12.556853961502));
#13172=CARTESIAN_POINT('Ctrl Pts',(83.9956695619749,25.2151332333942,-12.6679870794935));
#13173=CARTESIAN_POINT('Ctrl Pts',(85.4010382767464,23.364949738908,-12.7791201974851));
#13174=CARTESIAN_POINT('Ctrl Pts',(84.6088822566941,21.1807498790914,-12.8902533154767));
#13175=CARTESIAN_POINT('Ctrl Pts',(82.3442138703267,20.6615993349174,-13.0013864334682));
#13176=CARTESIAN_POINT('Ctrl Pts',(80.6797467613269,22.2826451179802,-13.1125195514598));
#13177=CARTESIAN_POINT('Ctrl Pts',(81.1388667406383,24.5602423238806,-13.2236526694513));
#13178=CARTESIAN_POINT('Ctrl Pts',(83.3013691324087,25.409844344426,-13.3347857874429));
#13179=CARTESIAN_POINT('Ctrl Pts',(85.1880466324256,24.0538619704037,-13.4459189054344));
#13180=CARTESIAN_POINT('Ctrl Pts',(85.0721377337693,21.7333436414648,-13.557052023426));
#13181=CARTESIAN_POINT('Ctrl Pts',(83.0597268226234,20.5721190669662,-13.6681851414176));
#13182=CARTESIAN_POINT('Ctrl Pts',(80.9926515725825,21.6329866828416,-13.7793182594091));
#13183=CARTESIAN_POINT('Ctrl Pts',(80.7627806117888,23.9449986917019,-13.8904513774007));
#13184=CARTESIAN_POINT('Ctrl Pts',(82.5805008911621,25.3921107031273,-14.0015844953923));
#13185=CARTESIAN_POINT('Ctrl Pts',(84.7821632663096,24.6498688464973,-14.1127176133838));
#13186=CARTESIAN_POINT('Ctrl Pts',(85.3527196747847,22.397602083335,-14.2238507313754));
#13187=CARTESIAN_POINT('Ctrl Pts',(83.7699744349188,20.6966736036812,-14.3349838493669));
#13188=CARTESIAN_POINT('Ctrl Pts',(81.4825182859858,21.1038400999306,-14.4461169673585));
#13189=CARTESIAN_POINT('Ctrl Pts',(80.5839211298768,23.2464467689522,-14.5572500853501));
#13190=CARTESIAN_POINT('Ctrl Pts',(81.8966144503262,25.1634956547744,-14.6683832033416));
#13191=CARTESIAN_POINT('Ctrl Pts',(84.2191696572937,25.1004281633947,-14.7795163213332));
#13192=CARTESIAN_POINT('Ctrl Pts',(85.4258928026212,23.1149661440179,-14.8906494393247));
#13193=CARTESIAN_POINT('Ctrl Pts',(84.4123433832198,21.0242825862308,-15.0017825573163));
#13194=CARTESIAN_POINT('Ctrl Pts',(82.1061616893797,20.7418533657775,-15.1129156753078));
#13195=CARTESIAN_POINT('Ctrl Pts',(80.6180560400795,22.5261688311867,-15.2240487932994));
#13196=CARTESIAN_POINT('Ctrl Pts',(81.3099991724782,24.7441532192698,-15.335181911291));
#13197=CARTESIAN_POINT('Ctrl Pts',(83.5486977451864,25.3658199574776,-15.4463150292825));
#13198=CARTESIAN_POINT('Ctrl Pts',(85.2852062155397,23.822195101775,-15.5574481472741));
#13199=CARTESIAN_POINT('Ctrl Pts',(84.9302046695978,21.5260650294792,-15.6685812652657));
#13200=CARTESIAN_POINT('Ctrl Pts',(82.8086025275965,20.5789380526202,-15.7797143832572));
#13201=CARTESIAN_POINT('Ctrl Pts',(80.862177498975,21.8476626671313,-15.8908475012488));
#13202=CARTESIAN_POINT('Ctrl Pts',(80.8723665552161,24.1710509563948,-16.0019806192403));
#13203=CARTESIAN_POINT('Ctrl Pts',(82.8298598776186,25.4226489294061,-16.1131137372319));
#13204=CARTESIAN_POINT('Ctrl Pts',(84.9430514056717,24.4569400344173,-16.2242468552234));
#13205=CARTESIAN_POINT('Ctrl Pts',(85.2779271552008,22.1577886838534,-16.335379973215));
#13206=CARTESIAN_POINT('Ctrl Pts',(83.5278718544653,20.6294494978248,-16.4465130912065));
#13207=CARTESIAN_POINT('Ctrl Pts',(81.2948519124425,21.270756926133,-16.5576462091981));
#13208=CARTESIAN_POINT('Ctrl Pts',(80.6221226182225,23.4946848360884,-16.6687793271897));
#13209=CARTESIAN_POINT('Ctrl Pts',(82.12637451265,25.2659591550417,-16.7799124451812));
#13210=CARTESIAN_POINT('Ctrl Pts',(84.4288972422666,24.9631356021949,-16.8910455631728));
#13211=CARTESIAN_POINT('Ctrl Pts',(85.4262517081314,22.8639849641985,-17.0021786811644));
#13212=CARTESIAN_POINT('Ctrl Pts',(84.1976566851383,20.8884152303676,-17.1133117991559));
#13213=CARTESIAN_POINT('Ctrl Pts',(82.656339145916,20.8620828587222,-17.1874005444836));
#13214=CARTESIAN_POINT('Ctrl Pts',(82.0504464477385,21.1778184465077,-17.2244449171475));
#13215=CARTESIAN_POINT('Ctrl Pts',(82.5032651029123,21.1400211999972,-5.92518502761751));
#13216=CARTESIAN_POINT('Ctrl Pts',(81.8848044607624,21.3051902779624,-5.96222940028136));
#13217=CARTESIAN_POINT('Ctrl Pts',(80.8363627669665,22.2985904105961,-6.03631814560907));
#13218=CARTESIAN_POINT('Ctrl Pts',(81.2373204918605,24.4411173205517,-6.14745126360063));
#13219=CARTESIAN_POINT('Ctrl Pts',(83.2546749659352,25.2606672752935,-6.25858438159218));
#13220=CARTESIAN_POINT('Ctrl Pts',(85.0373946220844,24.0131045499835,-6.36971749958376));
#13221=CARTESIAN_POINT('Ctrl Pts',(84.9561843853828,21.8373424170191,-6.4808506175753));
#13222=CARTESIAN_POINT('Ctrl Pts',(83.0842093017319,20.7261742931771,-6.59198373556687));
#13223=CARTESIAN_POINT('Ctrl Pts',(81.1353570388546,21.6958582941041,-6.70311685355843));
#13224=CARTESIAN_POINT('Ctrl Pts',(80.8930018887069,23.8592657828428,-6.81424997154998));
#13225=CARTESIAN_POINT('Ctrl Pts',(82.5791032362258,25.2361784018127,-6.92538308954154));
#13226=CARTESIAN_POINT('Ctrl Pts',(84.6504013517329,24.5664831205747,-7.0365162075331));
#13227=CARTESIAN_POINT('Ctrl Pts',(85.211199483728,22.4630654940639,-7.14764932552466));
#13228=CARTESIAN_POINT('Ctrl Pts',(83.7482146525832,20.8510791510673,-7.25878244351622));
#13229=CARTESIAN_POINT('Ctrl Pts',(81.6004374124557,21.2058658938257,-7.36991556150778));
#13230=CARTESIAN_POINT('Ctrl Pts',(80.7335933890972,23.2027167203527,-7.48104867949935));
#13231=CARTESIAN_POINT('Ctrl Pts',(81.9410546779104,25.0140322561575,-7.59218179749089));
#13232=CARTESIAN_POINT('Ctrl Pts',(84.1177040155997,24.9820266856548,-7.70331491548246));
#13233=CARTESIAN_POINT('Ctrl Pts',(85.2713868411497,23.1359920369145,-7.81444803347401));
#13234=CARTESIAN_POINT('Ctrl Pts',(84.3462069308205,21.1654922455966,-7.92558115146558));
#13235=CARTESIAN_POINT('Ctrl Pts',(82.1889255003257,20.8740060953579,-8.03671426945714));
#13236=CARTESIAN_POINT('Ctrl Pts',(80.77397135089,22.5283132756747,-8.14784738744869));
#13237=CARTESIAN_POINT('Ctrl Pts',(81.3963662491004,24.6143266960982,-8.25898050544026));
#13238=CARTESIAN_POINT('Ctrl Pts',(83.4864698683528,25.2228447926969,-8.3701136234318));
#13239=CARTESIAN_POINT('Ctrl Pts',(85.1313371199251,23.7969278408281,-8.48124674142338));
#13240=CARTESIAN_POINT('Ctrl Pts',(84.8255207491744,21.6416311642011,-8.59237985941492));
#13241=CARTESIAN_POINT('Ctrl Pts',(82.8489159377628,20.72956711,-8.70351297740649));
#13242=CARTESIAN_POINT('Ctrl Pts',(81.0105892063304,21.8954926005828,-8.81464609539804));
#13243=CARTESIAN_POINT('Ctrl Pts',(80.9930495359063,24.0723067358551,-8.92577921338961));
#13244=CARTESIAN_POINT('Ctrl Pts',(82.812349922923,25.2677035410137,-9.03691233138117));
#13245=CARTESIAN_POINT('Ctrl Pts',(84.8033950463649,24.3876088094334,-9.14804544937272));
#13246=CARTESIAN_POINT('Ctrl Pts',(85.1439020424116,22.23751987974,-9.25917856736428));
#13247=CARTESIAN_POINT('Ctrl Pts',(83.5222255060935,20.7852827670182,-9.37031168535585));
#13248=CARTESIAN_POINT('Ctrl Pts',(81.4225876319967,21.3600420363499,-9.48144480334739));
#13249=CARTESIAN_POINT('Ctrl Pts',(80.7666596434456,23.4357553821267,-9.59257792133896));
#13250=CARTESIAN_POINT('Ctrl Pts',(82.1547726526311,25.1126482510184,-9.70371103933051));
#13251=CARTESIAN_POINT('Ctrl Pts',(84.3164709979538,24.8559622875522,-9.81484415732209));
#13252=CARTESIAN_POINT('Ctrl Pts',(85.2732832701551,22.9006265885549,-9.92597727531363));
#13253=CARTESIAN_POINT('Ctrl Pts',(84.1494972179531,21.0362413470112,-10.0371103933052));
#13254=CARTESIAN_POINT('Ctrl Pts',(81.9736460681105,20.9691653174705,-10.1482435112967));
#13255=CARTESIAN_POINT('Ctrl Pts',(80.7371544336306,22.7607891222548,-10.2593766292883));
#13256=CARTESIAN_POINT('Ctrl Pts',(81.5717081262252,24.7713481376,-10.3705097472799));
#13257=CARTESIAN_POINT('Ctrl Pts',(83.7134907587191,25.1606996178304,-10.4816428652715));
#13258=CARTESIAN_POINT('Ctrl Pts',(85.2022585661105,23.5724937635141,-10.592775983263));
#13259=CARTESIAN_POINT('Ctrl Pts',(84.6754326537451,21.4603190836949,-10.7039091012546));
#13260=CARTESIAN_POINT('Ctrl Pts',(82.6151848322855,20.7573209797283,-10.8150422192461));
#13261=CARTESIAN_POINT('Ctrl Pts',(80.9071349984957,22.1069109861005,-10.9261753372377));
#13262=CARTESIAN_POINT('Ctrl Pts',(81.1145575884463,24.2738912096346,-11.0373084552292));
#13263=CARTESIAN_POINT('Ctrl Pts',(83.047611283741,25.2749560582416,-11.1484415732208));
#13264=CARTESIAN_POINT('Ctrl Pts',(84.9370892581942,24.1938915809481,-11.2595746912123));
#13265=CARTESIAN_POINT('Ctrl Pts',(85.0536669004577,22.0201305376561,-11.3707078092039));
#13266=CARTESIAN_POINT('Ctrl Pts',(83.2906477638809,20.7431845935875,-11.4818409271955));
#13267=CARTESIAN_POINT('Ctrl Pts',(81.2616163540157,21.5317649368565,-11.592974045187));
#13268=CARTESIAN_POINT('Ctrl Pts',(80.823622079069,23.6641317990833,-11.7041071631786));
#13269=CARTESIAN_POINT('Ctrl Pts',(82.3775345387585,25.1886590988163,-11.8152402811702));
#13270=CARTESIAN_POINT('Ctrl Pts',(84.5011518885781,24.7100394465299,-11.9263733991617));
#13271=CARTESIAN_POINT('Ctrl Pts',(85.2508559452084,22.6663243862826,-12.0375065171533));
#13272=CARTESIAN_POINT('Ctrl Pts',(83.9404880479573,20.9280023810537,-12.1486396351448));
#13273=CARTESIAN_POINT('Ctrl Pts',(81.7693484719668,21.086054149716,-12.2597727531364));
#13274=CARTESIAN_POINT('Ctrl Pts',(80.7245496124044,22.9958244927328,-12.3709058711279));
#13275=CARTESIAN_POINT('Ctrl Pts',(81.762332508424,24.9094164243469,-12.4820389891195));
#13276=CARTESIAN_POINT('Ctrl Pts',(83.9328774068518,25.0754352905006,-12.593172107111));
#13277=CARTESIAN_POINT('Ctrl Pts',(85.2496161848318,23.3419340904511,-12.7043052251026));
#13278=CARTESIAN_POINT('Ctrl Pts',(84.5074176864236,21.2954813524261,-12.8154383430942));
#13279=CARTESIAN_POINT('Ctrl Pts',(82.3855711900186,20.8090711698609,-12.9265714610857));
#13280=CARTESIAN_POINT('Ctrl Pts',(80.8260741241908,22.3278852867575,-13.0377045790773));
#13281=CARTESIAN_POINT('Ctrl Pts',(81.2562395847924,24.4618452433909,-13.1488376970688));
#13282=CARTESIAN_POINT('Ctrl Pts',(83.2823632111329,25.2578668956049,-13.2599708150604));
#13283=CARTESIAN_POINT('Ctrl Pts',(85.0500569129374,23.9873998961863,-13.371103933052));
#13284=CARTESIAN_POINT('Ctrl Pts',(84.9414578385667,21.8132256480966,-13.4822370510435));
#13285=CARTESIAN_POINT('Ctrl Pts',(83.0559601353062,20.7252339978527,-13.5933701690351));
#13286=CARTESIAN_POINT('Ctrl Pts',(81.1192455136393,21.7191977266905,-13.7045032870266));
#13287=CARTESIAN_POINT('Ctrl Pts',(80.9038714236746,23.885402107949,-13.8156364050182));
#13288=CARTESIAN_POINT('Ctrl Pts',(82.6069567095603,25.2412516309221,-13.9267695230098));
#13289=CARTESIAN_POINT('Ctrl Pts',(84.6697706849286,24.5458194464769,-14.0379026410013));
#13290=CARTESIAN_POINT('Ctrl Pts',(85.2043448078386,22.4355924617434,-14.1490357589929));
#13291=CARTESIAN_POINT('Ctrl Pts',(83.721415800604,20.8419334709107,-14.2601688769844));
#13292=CARTESIAN_POINT('Ctrl Pts',(81.5782186576973,21.2234219081233,-14.371301994976));
#13293=CARTESIAN_POINT('Ctrl Pts',(80.7362917606528,23.2309045405497,-14.4824351129676));
#13294=CARTESIAN_POINT('Ctrl Pts',(81.9661997417136,25.0270542489596,-14.5935682309591));
#13295=CARTESIAN_POINT('Ctrl Pts',(84.1422824115993,24.9679641250252,-14.7047013489507));
#13296=CARTESIAN_POINT('Ctrl Pts',(85.2729032536867,23.1077157747943,-14.8158344669422));
#13297=CARTESIAN_POINT('Ctrl Pts',(84.3232735871819,21.1488817093362,-14.9269675849338));
#13298=CARTESIAN_POINT('Ctrl Pts',(82.1625318306384,20.8842639597758,-15.0381007029254));
#13299=CARTESIAN_POINT('Ctrl Pts',(80.7682739440287,22.5560511148183,-15.1492338209169));
#13300=CARTESIAN_POINT('Ctrl Pts',(81.4165795061277,24.6341577512094,-15.2603669389085));
#13301=CARTESIAN_POINT('Ctrl Pts',(83.5140939818022,25.216618917859,-15.3715000569));
#13302=CARTESIAN_POINT('Ctrl Pts',(85.1410891021372,23.7703431577729,-15.4826331748916));
#13303=CARTESIAN_POINT('Ctrl Pts',(84.8084758193231,21.6190191146948,-15.5937662928831));
#13304=CARTESIAN_POINT('Ctrl Pts',(82.8206730580578,20.7316229424355,-15.7048994108747));
#13305=CARTESIAN_POINT('Ctrl Pts',(80.9969998207942,21.9203351152235,-15.8160325288663));
#13306=CARTESIAN_POINT('Ctrl Pts',(81.006546301602,24.0971983288573,-15.9271656468579));
#13307=CARTESIAN_POINT('Ctrl Pts',(82.840589807874,25.2698639561642,-16.0382987648494));
#13308=CARTESIAN_POINT('Ctrl Pts',(84.8205123727065,24.365057739186,-16.1494318828409));
#13309=CARTESIAN_POINT('Ctrl Pts',(85.1342690975971,22.210902955525,-16.2605650008325));
#13310=CARTESIAN_POINT('Ctrl Pts',(83.4945814811962,20.7789488704525,-16.371698118824));
#13311=CARTESIAN_POINT('Ctrl Pts',(81.4023875119133,21.379812082067,-16.4828312368156));
#13312=CARTESIAN_POINT('Ctrl Pts',(80.7720840623829,23.4634874106061,-16.5939643548072));
#13313=CARTESIAN_POINT('Ctrl Pts',(82.1814699270488,25.1230558624233,-16.7050974727988));
#13314=CARTESIAN_POINT('Ctrl Pts',(84.3387834728816,24.8393299542485,-16.8162305907903));
#13315=CARTESIAN_POINT('Ctrl Pts',(85.2732395247293,22.8725627871564,-16.9273637087819));
#13316=CARTESIAN_POINT('Ctrl Pts',(84.122126160525,21.0215828629579,-17.0384968267734));
#13317=CARTESIAN_POINT('Ctrl Pts',(82.6780122054164,20.996911149053,-17.1125855721011));
#13318=CARTESIAN_POINT('Ctrl Pts',(82.1103302849355,21.2927347913867,-17.149629944765));
#13319=CARTESIAN_POINT('Ctrl Pts',(82.5367004230132,21.2652167256662,-5.85037005523502));
#13320=CARTESIAN_POINT('Ctrl Pts',(81.9598684839428,21.4192682416784,-5.88741442789887));
#13321=CARTESIAN_POINT('Ctrl Pts',(80.9819975993346,22.3458024230419,-5.96150317322658));
#13322=CARTESIAN_POINT('Ctrl Pts',(81.3559667837468,24.3441154404782,-6.07263629121814));
#13323=CARTESIAN_POINT('Ctrl Pts',(83.2375327456932,25.1085013323846,-6.1837694092097));
#13324=CARTESIAN_POINT('Ctrl Pts',(84.9002572037943,23.9449122906456,-6.29490252720126));
#13325=CARTESIAN_POINT('Ctrl Pts',(84.8245132435218,21.9156011193624,-6.40603564519281));
#13326=CARTESIAN_POINT('Ctrl Pts',(83.0785411576668,20.8792259326071,-6.51716876318437));
#13327=CARTESIAN_POINT('Ctrl Pts',(81.2608665100943,21.7836403195853,-6.62830188117594));
#13328=CARTESIAN_POINT('Ctrl Pts',(81.0348243310523,23.801428440088,-6.73943499916749));
#13329=CARTESIAN_POINT('Ctrl Pts',(82.6074338771949,25.0856608096207,-6.85056811715905));
#13330=CARTESIAN_POINT('Ctrl Pts',(84.5393125238417,24.461042844733,-6.96170123515062));
#13331=CARTESIAN_POINT('Ctrl Pts',(85.0623632272481,22.499206657458,-7.07283435314217));
#13332=CARTESIAN_POINT('Ctrl Pts',(83.6978521824609,20.9957234208314,-7.18396747113373));
#13333=CARTESIAN_POINT('Ctrl Pts',(81.6946422355719,21.3266294006694,-7.29510058912529));
#13334=CARTESIAN_POINT('Ctrl Pts',(80.8861456477742,23.1890718194718,-7.40623370711685));
#13335=CARTESIAN_POINT('Ctrl Pts',(82.01233248831,24.8784673631472,-7.5173668251084));
#13336=CARTESIAN_POINT('Ctrl Pts',(84.0424711463996,24.848616093663,-7.62849994309996));
#13337=CARTESIAN_POINT('Ctrl Pts',(85.1184993622307,23.1268383871266,-7.73963306109152));
#13338=CARTESIAN_POINT('Ctrl Pts',(84.2555934870742,21.2889733103571,-7.85076617908308));
#13339=CARTESIAN_POINT('Ctrl Pts',(82.2435190786735,21.017107148155,-7.96189929707465));
#13340=CARTESIAN_POINT('Ctrl Pts',(80.9238057613034,22.560062598518,-8.0730324150662));
#13341=CARTESIAN_POINT('Ctrl Pts',(81.5043071409126,24.5056660601172,-8.18416553305777));
#13342=CARTESIAN_POINT('Ctrl Pts',(83.4537254892822,25.0732246882625,-8.29529865104932));
#13343=CARTESIAN_POINT('Ctrl Pts',(84.9878764142944,23.7432864767692,-8.40643176904088));
#13344=CARTESIAN_POINT('Ctrl Pts',(84.7026446014396,21.7330632280773,-8.51756488703244));
#13345=CARTESIAN_POINT('Ctrl Pts',(82.8590854346367,20.8823903782863,-8.628698005024));
#13346=CARTESIAN_POINT('Ctrl Pts',(81.1444968240326,21.9698372030455,-8.73983112301556));
#13347=CARTESIAN_POINT('Ctrl Pts',(81.12813775215,24.0001295661618,-8.85096424100711));
#13348=CARTESIAN_POINT('Ctrl Pts',(82.8249806851885,25.1150639857251,-8.96209735899869));
#13349=CARTESIAN_POINT('Ctrl Pts',(84.6820081838812,24.2942085973882,-9.07323047699023));
#13350=CARTESIAN_POINT('Ctrl Pts',(84.9995955894661,22.2888425611964,-9.18436359498179));
#13351=CARTESIAN_POINT('Ctrl Pts',(83.4870744082675,20.9343558038673,-9.29549671297336));
#13352=CARTESIAN_POINT('Ctrl Pts',(81.5287635575549,21.4704279178093,-9.40662983096491));
#13353=CARTESIAN_POINT('Ctrl Pts',(80.9169862062732,23.4064246047392,-9.51776294895648));
#13354=CARTESIAN_POINT('Ctrl Pts',(82.2116650656326,24.970445496697,-9.62889606694802));
#13355=CARTESIAN_POINT('Ctrl Pts',(84.2278590854866,24.7310371140978,-9.74002918493959));
#13356=CARTESIAN_POINT('Ctrl Pts',(85.1202681422402,22.9073154317199,-9.85116230293115));
#13357=CARTESIAN_POINT('Ctrl Pts',(84.0721243422749,21.1684223142607,-9.9622954209227));
#13358=CARTESIAN_POINT('Ctrl Pts',(82.0427301458566,21.1058611849855,-10.0734285389143));
#13359=CARTESIAN_POINT('Ctrl Pts',(80.8894669977249,22.7768904517888,-10.1845616569058));
#13360=CARTESIAN_POINT('Ctrl Pts',(81.6678467230445,24.6521183586212,-10.2956947748974));
#13361=CARTESIAN_POINT('Ctrl Pts',(83.6654655604762,25.0152625168986,-10.406827892889));
#13362=CARTESIAN_POINT('Ctrl Pts',(85.0540241244907,23.5339590997506,-10.5179610108805));
#13363=CARTESIAN_POINT('Ctrl Pts',(84.5626589641695,21.5639552980856,-10.6290941288721));
#13364=CARTESIAN_POINT('Ctrl Pts',(82.6410868141831,20.9082761297812,-10.7402272468636));
#13365=CARTESIAN_POINT('Ctrl Pts',(81.0480061385414,22.1670249769504,-10.8513603648552));
#13366=CARTESIAN_POINT('Ctrl Pts',(81.2414670746365,24.188145350792,-10.9624934828467));
#13367=CARTESIAN_POINT('Ctrl Pts',(83.0444065592057,25.1218283346434,-11.0736266008383));
#13368=CARTESIAN_POINT('Ctrl Pts',(84.8067034129645,24.1135305122798,-11.1847597188299));
#13369=CARTESIAN_POINT('Ctrl Pts',(84.9154341920251,22.0860857369438,-11.2958928368214));
#13370=CARTESIAN_POINT('Ctrl Pts',(83.2710842077889,20.8950912664717,-11.407025954813));
#13371=CARTESIAN_POINT('Ctrl Pts',(81.3786272868141,21.6305921173251,-11.5181590728045));
#13372=CARTESIAN_POINT('Ctrl Pts',(80.9701144895549,23.6194289617716,-11.6292921907961));
#13373=CARTESIAN_POINT('Ctrl Pts',(82.4194328069704,25.0413400399184,-11.7404253087876));
#13374=CARTESIAN_POINT('Ctrl Pts',(84.4001090703485,24.5949363671707,-11.8515584267792));
#13375=CARTESIAN_POINT('Ctrl Pts',(85.0993504047878,22.6887841551048,-11.9626915447708));
#13376=CARTESIAN_POINT('Ctrl Pts',(83.8771836191383,21.0674689336232,-12.0738246627623));
#13377=CARTESIAN_POINT('Ctrl Pts',(81.8521838596429,21.2148822077712,-12.1849577807539));
#13378=CARTESIAN_POINT('Ctrl Pts',(80.8777106094051,22.9961055469186,-12.2960908987455));
#13379=CARTESIAN_POINT('Ctrl Pts',(81.8456401419364,24.7808932428103,-12.407224016737));
#13380=CARTESIAN_POINT('Ctrl Pts',(83.8700852517286,24.935737347607,-12.5183571347286));
#13381=CARTESIAN_POINT('Ctrl Pts',(85.0981940929171,23.3189184419942,-12.6294902527201));
#13382=CARTESIAN_POINT('Ctrl Pts',(84.4059531161532,21.4102128257608,-12.7406233707117));
#13383=CARTESIAN_POINT('Ctrl Pts',(82.4269285097103,20.9565430048045,-12.8517564887032));
#13384=CARTESIAN_POINT('Ctrl Pts',(80.9724014870548,22.3731254555347,-12.9628896066948));
#13385=CARTESIAN_POINT('Ctrl Pts',(81.3736124289465,24.3634481629012,-13.0740227246864));
#13386=CARTESIAN_POINT('Ctrl Pts',(83.2633572898572,25.1058894467837,-13.1851558426779));
#13387=CARTESIAN_POINT('Ctrl Pts',(84.9120671934491,23.9209378219689,-13.2962889606695));
#13388=CARTESIAN_POINT('Ctrl Pts',(84.810777943364,21.8931076547286,-13.407422078661));
#13389=CARTESIAN_POINT('Ctrl Pts',(83.052193447989,20.8783489287391,-13.5185551966526));
#13390=CARTESIAN_POINT('Ctrl Pts',(81.2458394546959,21.8054087705393,-13.6296883146441));
#13391=CARTESIAN_POINT('Ctrl Pts',(81.0449622355604,23.825805524196,-13.7408214326357));
#13392=CARTESIAN_POINT('Ctrl Pts',(82.6334125279584,25.0903925587169,-13.8519545506273));
#13393=CARTESIAN_POINT('Ctrl Pts',(84.5573781035476,24.4417700464565,-13.9630876686188));
#13394=CARTESIAN_POINT('Ctrl Pts',(85.0559699408925,22.4735828401516,-14.0742207866104));
#13395=CARTESIAN_POINT('Ctrl Pts',(83.6728571662892,20.9871933381401,-14.185353904602));
#13396=CARTESIAN_POINT('Ctrl Pts',(81.6739190294089,21.343003716316,-14.2964870225935));
#13397=CARTESIAN_POINT('Ctrl Pts',(80.8886623914287,23.2153623121472,-14.4076201405851));
#13398=CARTESIAN_POINT('Ctrl Pts',(82.0357850331013,24.8906128431449,-14.5187532585766));
#13399=CARTESIAN_POINT('Ctrl Pts',(84.0653951659045,24.8355000866556,-14.6298863765682));
#13400=CARTESIAN_POINT('Ctrl Pts',(85.1199137047525,23.1004654055706,-14.7410194945597));
#13401=CARTESIAN_POINT('Ctrl Pts',(84.2342037911438,21.2734808324417,-14.8521526125513));
#13402=CARTESIAN_POINT('Ctrl Pts',(82.218901971897,21.0266745537741,-14.9632857305429));
#13403=CARTESIAN_POINT('Ctrl Pts',(80.918491847978,22.5859333984499,-15.0744188485344));
#13404=CARTESIAN_POINT('Ctrl Pts',(81.5231598397772,24.524162283149,-15.185551966526));
#13405=CARTESIAN_POINT('Ctrl Pts',(83.479490218418,25.0674178782403,-15.2966850845176));
#13406=CARTESIAN_POINT('Ctrl Pts',(84.9969719887346,23.7184912137708,-15.4078182025091));
#13407=CARTESIAN_POINT('Ctrl Pts',(84.6867469690484,21.7119731999103,-15.5189513205007));
#13408=CARTESIAN_POINT('Ctrl Pts',(82.8327435885193,20.8843078322508,-15.6300844384922));
#13409=CARTESIAN_POINT('Ctrl Pts',(81.1318221426133,21.9930075633158,-15.7412175564838));
#13410=CARTESIAN_POINT('Ctrl Pts',(81.140726047988,24.0233457013197,-15.8523506744754));
#13411=CARTESIAN_POINT('Ctrl Pts',(82.8513197381292,25.1170789829222,-15.9634837924669));
#13412=CARTESIAN_POINT('Ctrl Pts',(84.6979733397415,24.2731754439547,-16.0746169104585));
#13413=CARTESIAN_POINT('Ctrl Pts',(84.9906110399931,22.2640172271967,-16.18575002845));
#13414=CARTESIAN_POINT('Ctrl Pts',(83.4612911079274,20.9284482430803,-16.2968831464416));
#13415=CARTESIAN_POINT('Ctrl Pts',(81.509923111384,21.4888672380009,-16.4080162644331));
#13416=CARTESIAN_POINT('Ctrl Pts',(80.9220455065434,23.4322899851238,-16.5191493824247));
#13417=CARTESIAN_POINT('Ctrl Pts',(82.2365653414475,24.980152569805,-16.6302825004163));
#13418=CARTESIAN_POINT('Ctrl Pts',(84.2486697034967,24.7155243063022,-16.7414156184078));
#13419=CARTESIAN_POINT('Ctrl Pts',(85.1202273413273,22.8811406101142,-16.8525487363994));
#13420=CARTESIAN_POINT('Ctrl Pts',(84.0465956359117,21.1547504955482,-16.9636818543909));
#13421=CARTESIAN_POINT('Ctrl Pts',(82.6996852649168,21.1317394393839,-17.0377705997186));
#13422=CARTESIAN_POINT('Ctrl Pts',(82.1702141221325,21.4076511362656,-17.0748149723825));
#13423=CARTESIAN_POINT('Ctrl Pts',(82.5701357431142,21.3904122513352,-5.77555508285253));
#13424=CARTESIAN_POINT('Ctrl Pts',(82.0349325071233,21.5333462053945,-5.81259945551638));
#13425=CARTESIAN_POINT('Ctrl Pts',(81.1276324317026,22.3930144354877,-5.88668820084408));
#13426=CARTESIAN_POINT('Ctrl Pts',(81.4746130756331,24.2471135604047,-5.99782131883566));
#13427=CARTESIAN_POINT('Ctrl Pts',(83.2203905254512,24.9563353894757,-6.1089544368272));
#13428=CARTESIAN_POINT('Ctrl Pts',(84.7631197855041,23.8767200313077,-6.22008755481878));
#13429=CARTESIAN_POINT('Ctrl Pts',(84.6928421016609,21.9938598217058,-6.33122067281032));
#13430=CARTESIAN_POINT('Ctrl Pts',(83.0728730136016,21.0322775720369,-6.44235379080189));
#13431=CARTESIAN_POINT('Ctrl Pts',(81.3863759813341,21.8714223450666,-6.55348690879345));
#13432=CARTESIAN_POINT('Ctrl Pts',(81.1766467733975,23.7435910973332,-6.66462002678501));
#13433=CARTESIAN_POINT('Ctrl Pts',(82.6357645181641,24.9351432174288,-6.77575314477656));
#13434=CARTESIAN_POINT('Ctrl Pts',(84.4282236959502,24.3556025688913,-6.88688626276812));
#13435=CARTESIAN_POINT('Ctrl Pts',(84.9135269707684,22.5353478208521,-6.99801938075968));
#13436=CARTESIAN_POINT('Ctrl Pts',(83.6474897123384,21.1403676905955,-7.10915249875123));
#13437=CARTESIAN_POINT('Ctrl Pts',(81.7888470586882,21.447392907513,-7.22028561674281));
#13438=CARTESIAN_POINT('Ctrl Pts',(81.038697906451,23.175426918591,-7.33141873473436));
#13439=CARTESIAN_POINT('Ctrl Pts',(82.0836102987095,24.7429024701368,-7.44255185272592));
#13440=CARTESIAN_POINT('Ctrl Pts',(83.9672382771997,24.7152055016712,-7.55368497071747));
#13441=CARTESIAN_POINT('Ctrl Pts',(84.9656118833117,23.1176847373386,-7.66481808870904));
#13442=CARTESIAN_POINT('Ctrl Pts',(84.1649800433279,21.4124543751176,-7.7759512067006));
#13443=CARTESIAN_POINT('Ctrl Pts',(82.2981126570216,21.1602082009521,-7.88708432469216));
#13444=CARTESIAN_POINT('Ctrl Pts',(81.0736401717165,22.5918119213613,-7.99821744268371));
#13445=CARTESIAN_POINT('Ctrl Pts',(81.6122480327251,24.3970054241362,-8.10935056067527));
#13446=CARTESIAN_POINT('Ctrl Pts',(83.4209811102115,24.9236045838281,-8.22048367866682));
#13447=CARTESIAN_POINT('Ctrl Pts',(84.8444157086637,23.6896451127104,-8.3316167966584));
#13448=CARTESIAN_POINT('Ctrl Pts',(84.5797684537048,21.8244952919535,-8.44274991464993));
#13449=CARTESIAN_POINT('Ctrl Pts',(82.8692549315105,21.0352136465726,-8.55388303264152));
#13450=CARTESIAN_POINT('Ctrl Pts',(81.2784044417347,22.0441818055082,-8.66501615063305));
#13451=CARTESIAN_POINT('Ctrl Pts',(81.263225968394,23.9279523964684,-8.77614926862464));
#13452=CARTESIAN_POINT('Ctrl Pts',(82.8376114474537,24.9624244304365,-8.88728238661618));
#13453=CARTESIAN_POINT('Ctrl Pts',(84.5606213213977,24.2008083853429,-8.99841550460775));
#13454=CARTESIAN_POINT('Ctrl Pts',(84.8552891365203,22.3401652426527,-9.10954862259931));
#13455=CARTESIAN_POINT('Ctrl Pts',(83.4519233104416,21.0834288407163,-9.22068174059086));
#13456=CARTESIAN_POINT('Ctrl Pts',(81.634939483113,21.5808137992688,-9.33181485858243));
#13457=CARTESIAN_POINT('Ctrl Pts',(81.0673127691008,23.3770938273516,-9.44294797657398));
#13458=CARTESIAN_POINT('Ctrl Pts',(82.2685574786339,24.8282427423756,-9.55408109456554));
#13459=CARTESIAN_POINT('Ctrl Pts',(84.1392471730195,24.6061119406434,-9.6652142125571));
#13460=CARTESIAN_POINT('Ctrl Pts',(84.9672530143251,22.9140042748849,-9.77634733054867));
#13461=CARTESIAN_POINT('Ctrl Pts',(83.9947514665968,21.3006032815102,-9.88748044854021));
#13462=CARTESIAN_POINT('Ctrl Pts',(82.1118142236025,21.2425570525006,-9.99861356653178));
#13463=CARTESIAN_POINT('Ctrl Pts',(81.041779561819,22.7929917813227,-10.1097466845233));
#13464=CARTESIAN_POINT('Ctrl Pts',(81.7639853198639,24.5328885796424,-10.2208798025149));
#13465=CARTESIAN_POINT('Ctrl Pts',(83.6174403622332,24.8698254159668,-10.3320129205065));
#13466=CARTESIAN_POINT('Ctrl Pts',(84.9057896828708,23.4954244359871,-10.443146038498));
#13467=CARTESIAN_POINT('Ctrl Pts',(84.4498852745941,21.6675915124763,-10.5542791564896));
#13468=CARTESIAN_POINT('Ctrl Pts',(82.6669887960806,21.0592312798342,-10.6654122744811));
#13469=CARTESIAN_POINT('Ctrl Pts',(81.1888772785873,22.2271389678003,-10.7765453924727));
#13470=CARTESIAN_POINT('Ctrl Pts',(81.3683765608268,24.1023994919494,-10.8876785104643));
#13471=CARTESIAN_POINT('Ctrl Pts',(83.0412018346701,24.9687006110452,-10.9988116284558));
#13472=CARTESIAN_POINT('Ctrl Pts',(84.6763175677353,24.0331694436115,-11.1099447464474));
#13473=CARTESIAN_POINT('Ctrl Pts',(84.7772014835923,22.1520409362315,-11.2210778644389));
#13474=CARTESIAN_POINT('Ctrl Pts',(83.2515206516971,21.046997939356,-11.3322109824305));
#13475=CARTESIAN_POINT('Ctrl Pts',(81.4956382196122,21.7294192977939,-11.4433441004221));
#13476=CARTESIAN_POINT('Ctrl Pts',(81.116606900041,23.5747261244599,-11.5544772184136));
#13477=CARTESIAN_POINT('Ctrl Pts',(82.4613310751823,24.8940209810205,-11.6656103364052));
#13478=CARTESIAN_POINT('Ctrl Pts',(84.2990662521189,24.4798332878116,-11.7767434543967));
#13479=CARTESIAN_POINT('Ctrl Pts',(84.9478448643671,22.7112439239271,-11.8878765723883));
#13480=CARTESIAN_POINT('Ctrl Pts',(83.8138791903196,21.2069354861927,-11.9990096903798));
#13481=CARTESIAN_POINT('Ctrl Pts',(81.9350192473189,21.3437102658265,-12.1101428083714));
#13482=CARTESIAN_POINT('Ctrl Pts',(81.0308716064059,22.9963866011044,-12.221275926363));
#13483=CARTESIAN_POINT('Ctrl Pts',(81.9289477754486,24.6523700612737,-12.3324090443545));
#13484=CARTESIAN_POINT('Ctrl Pts',(83.8072930966055,24.7960394047134,-12.4435421623461));
#13485=CARTESIAN_POINT('Ctrl Pts',(84.9467720010023,23.2959027935373,-12.5546752803376));
#13486=CARTESIAN_POINT('Ctrl Pts',(84.3044885458827,21.5249442990955,-12.6658083983292));
#13487=CARTESIAN_POINT('Ctrl Pts',(82.4682858294022,21.1040148397481,-12.7769415163207));
#13488=CARTESIAN_POINT('Ctrl Pts',(81.1187288499188,22.418365624312,-12.8880746343123));
#13489=CARTESIAN_POINT('Ctrl Pts',(81.4909852731006,24.2650510824115,-12.9992077523039));
#13490=CARTESIAN_POINT('Ctrl Pts',(83.2443513685815,24.9539119979626,-13.1103408702954));
#13491=CARTESIAN_POINT('Ctrl Pts',(84.7740774739608,23.8544757477516,-13.221473988287));
#13492=CARTESIAN_POINT('Ctrl Pts',(84.6800980481614,21.9729896613604,-13.3326071062786));
#13493=CARTESIAN_POINT('Ctrl Pts',(83.0484267606719,21.0314638596256,-13.4437402242701));
#13494=CARTESIAN_POINT('Ctrl Pts',(81.3724333957525,21.8916198143882,-13.5548733422617));
#13495=CARTESIAN_POINT('Ctrl Pts',(81.1860530474464,23.7662089404431,-13.6660064602532));
#13496=CARTESIAN_POINT('Ctrl Pts',(82.6598683463564,24.9395334865117,-13.7771395782448));
#13497=CARTESIAN_POINT('Ctrl Pts',(84.4449855221666,24.337720646436,-13.8882726962363));
#13498=CARTESIAN_POINT('Ctrl Pts',(84.9075950739464,22.51157321856,-13.9994058142279));
#13499=CARTESIAN_POINT('Ctrl Pts',(83.6242985319745,21.1324532053695,-14.1105389322195));
#13500=CARTESIAN_POINT('Ctrl Pts',(81.7696194011205,21.4625855245088,-14.221672050211));
#13501=CARTESIAN_POINT('Ctrl Pts',(81.0410330222045,23.1998200837446,-14.3328051682026));
#13502=CARTESIAN_POINT('Ctrl Pts',(82.1053703244889,24.7541714373302,-14.4439382861941));
#13503=CARTESIAN_POINT('Ctrl Pts',(83.9885079202099,24.7030360482859,-14.5550714041857));
#13504=CARTESIAN_POINT('Ctrl Pts',(84.9669241558181,23.093215036347,-14.6662045221773));
#13505=CARTESIAN_POINT('Ctrl Pts',(84.145133995106,21.3980799555471,-14.7773376401688));
#13506=CARTESIAN_POINT('Ctrl Pts',(82.2752721131558,21.1690851477724,-14.8884707581604));
#13507=CARTESIAN_POINT('Ctrl Pts',(81.0687097519271,22.6158156820815,-14.9996038761519));
#13508=CARTESIAN_POINT('Ctrl Pts',(81.6297401734268,24.4141668150886,-15.1107369941435));
#13509=CARTESIAN_POINT('Ctrl Pts',(83.4448864550338,24.9182168386216,-15.2218701121351));
#13510=CARTESIAN_POINT('Ctrl Pts',(84.8528548753323,23.6666392697687,-15.3330032301266));
#13511=CARTESIAN_POINT('Ctrl Pts',(84.5650181187735,21.8049272851258,-15.4441363481182));
#13512=CARTESIAN_POINT('Ctrl Pts',(82.8448141189808,21.0369927220661,-15.5552694661097));
#13513=CARTESIAN_POINT('Ctrl Pts',(81.2666444644324,22.065680011408,-15.6664025841013));
#13514=CARTESIAN_POINT('Ctrl Pts',(81.274905794374,23.9494930737822,-15.7775357020929));
#13515=CARTESIAN_POINT('Ctrl Pts',(82.8620496683843,24.9642940096802,-15.8886688200844));
#13516=CARTESIAN_POINT('Ctrl Pts',(84.5754343067765,24.1812931487234,-15.999801938076));
#13517=CARTESIAN_POINT('Ctrl Pts',(84.8469529823893,22.3171314988683,-16.1109350560675));
#13518=CARTESIAN_POINT('Ctrl Pts',(83.4280007346583,21.077947615708,-16.2220681740591));
#13519=CARTESIAN_POINT('Ctrl Pts',(81.6174587108549,21.5979223939348,-16.3332012920506));
#13520=CARTESIAN_POINT('Ctrl Pts',(81.0720069507038,23.4010925596415,-16.4443344100422));
#13521=CARTESIAN_POINT('Ctrl Pts',(82.2916607558463,24.8372492771867,-16.5554675280338));
#13522=CARTESIAN_POINT('Ctrl Pts',(84.1585559341117,24.5917186583559,-16.6666006460253));
#13523=CARTESIAN_POINT('Ctrl Pts',(84.9672151579253,22.889718433072,-16.7777337640169));
#13524=CARTESIAN_POINT('Ctrl Pts',(83.9710651112984,21.2879181281384,-16.8888668820084));
#13525=CARTESIAN_POINT('Ctrl Pts',(82.7213583244171,21.2665677297147,-16.9629556273361));
#13526=CARTESIAN_POINT('Ctrl Pts',(82.2300979593295,21.5225674811446,-17.));
#13527=CARTESIAN_POINT('Ctrl Pts',(81.3361556106367,23.000944168981,-6.62148036339021));
#13528=CARTESIAN_POINT('Ctrl Pts',(81.335036709732,23.2166368660648,-6.63586025118848));
#13529=CARTESIAN_POINT('Ctrl Pts',(81.3739566403903,23.4319424195808,-6.65024013898675));
#13530=CARTESIAN_POINT('Ctrl Pts',(81.4547879321813,23.6301549919714,-6.66462002678502));
#13531=CARTESIAN_POINT('Ctrl Pts',(81.6630193549864,24.1407751373651,-6.70166439944887));
#13532=CARTESIAN_POINT('Ctrl Pts',(82.1493919365753,24.537959177397,-6.73870877211272));
#13533=CARTESIAN_POINT('Ctrl Pts',(82.6913214236674,24.6399610893233,-6.77575314477657));
#13534=CARTESIAN_POINT('Ctrl Pts',(83.2332509107595,24.7419630012497,-6.81279751744043));
#13535=CARTESIAN_POINT('Ctrl Pts',(83.8307373033549,24.5487827850705,-6.84984189010428));
#13536=CARTESIAN_POINT('Ctrl Pts',(84.210364378789,24.1488168856411,-6.88688626276813));
#13537=CARTESIAN_POINT('Ctrl Pts',(84.589991454223,23.7488509862116,-6.92393063543199));
#13538=CARTESIAN_POINT('Ctrl Pts',(84.7517592124957,23.1420994035318,-6.96097500809584));
#13539=CARTESIAN_POINT('Ctrl Pts',(84.6216368818937,22.6062269238159,-6.99801938075969));
#13540=CARTESIAN_POINT('Ctrl Pts',(84.4915145512917,22.0703544440999,-7.03506375342354));
#13541=CARTESIAN_POINT('Ctrl Pts',(84.069502131815,21.6053610673477,-7.07210812608739));
#13542=CARTESIAN_POINT('Ctrl Pts',(83.5487221464684,21.4240352484578,-7.10915249875125));
#13543=CARTESIAN_POINT('Ctrl Pts',(83.0279421611216,21.2427094295679,-7.1461968714151));
#13544=CARTESIAN_POINT('Ctrl Pts',(82.4083946099049,21.3450511685405,-7.18324124407896));
#13545=CARTESIAN_POINT('Ctrl Pts',(81.9735959755904,21.6842277065397,-7.22028561674282));
#13546=CARTESIAN_POINT('Ctrl Pts',(81.5776803526215,21.9930724906318,-7.25401719895862));
#13547=CARTESIAN_POINT('Ctrl Pts',(81.3349478237242,22.4982869634183,-7.28774878117441));
#13548=CARTESIAN_POINT('Ctrl Pts',(81.3317908287134,23.0008588708997,-7.32148036339021));
#13549=CARTESIAN_POINT('Ctrl Pts',(82.4698297828114,21.0148256743283,-6.));
#13550=CARTESIAN_POINT('Ctrl Pts',(82.4011651263259,21.0402496509185,-6.));
#13551=CARTESIAN_POINT('Ctrl Pts',(82.3342038137343,21.0695633264578,-6.));
#13552=CARTESIAN_POINT('Ctrl Pts',(82.269134779623,21.1024726694379,-6.));
#13553=CARTESIAN_POINT('Ctrl Pts',(82.2022546944968,21.1362979703666,-6.));
#13554=CARTESIAN_POINT('Ctrl Pts',(82.1373729168602,21.1739225674446,-6.));
#13555=CARTESIAN_POINT('Ctrl Pts',(82.0747258152859,21.2150718339324,-6.));
#13556=CARTESIAN_POINT('Ctrl Pts',(82.0217930857579,21.2498402899109,-6.));
#13557=CARTESIAN_POINT('Ctrl Pts',(81.9704560596044,21.2871261118042,-6.));
#13558=CARTESIAN_POINT('Ctrl Pts',(81.9208800568393,21.3267816542417,-6.));
#13559=CARTESIAN_POINT('Ctrl Pts',(81.8988503402036,21.3444030903036,-6.));
#13560=CARTESIAN_POINT('Ctrl Pts',(81.8771686550144,21.3624926256576,-6.));
#13561=CARTESIAN_POINT('Ctrl Pts',(81.8558510604217,21.3810380294145,-6.));
#13562=CARTESIAN_POINT('Ctrl Pts',(81.8441385158822,21.3912274467317,-6.));
#13563=CARTESIAN_POINT('Ctrl Pts',(81.832535898607,21.4015544856012,-6.));
#13564=CARTESIAN_POINT('Ctrl Pts',(81.8210460063917,21.4120171590794,-6.));
#13565=CARTESIAN_POINT('Ctrl Pts',(81.8104524191136,21.4216636590269,-6.));
#13566=CARTESIAN_POINT('Ctrl Pts',(81.7999532220216,21.4314269732589,-6.));
#13567=CARTESIAN_POINT('Ctrl Pts',(81.7895664958216,21.44129008872,-6.));
#13568=CARTESIAN_POINT('Ctrl Pts',(81.7364817397298,21.4916987611424,-6.));
#13569=CARTESIAN_POINT('Ctrl Pts',(81.6862369782681,21.5447958399209,-6.));
#13570=CARTESIAN_POINT('Ctrl Pts',(81.6390508775578,21.6003218536055,-6.));
#13571=CARTESIAN_POINT('Ctrl Pts',(81.5922309148136,21.6554170162255,-6.));
#13572=CARTESIAN_POINT('Ctrl Pts',(81.5484218215863,21.7129044490147,-6.));
#13573=CARTESIAN_POINT('Ctrl Pts',(81.5078820049586,21.7725549136341,-6.));
#13574=CARTESIAN_POINT('Ctrl Pts',(81.4741935898231,21.822124195942,-6.));
#13575=CARTESIAN_POINT('Ctrl Pts',(81.4427634303418,21.8731878200883,-6.));
#13576=CARTESIAN_POINT('Ctrl Pts',(81.4137674155173,21.9256207131518,-6.));
#13577=CARTESIAN_POINT('Ctrl Pts',(81.4016612624094,21.9475120190833,-6.));
#13578=CARTESIAN_POINT('Ctrl Pts',(81.3899797398811,21.9696420487289,-6.));
#13579=CARTESIAN_POINT('Ctrl Pts',(81.3787370903759,21.9920017823975,-6.));
#13580=CARTESIAN_POINT('Ctrl Pts',(81.3735362822328,22.0023453126204,-6.));
#13581=CARTESIAN_POINT('Ctrl Pts',(81.3684294032715,22.0127379983886,-6.));
#13582=CARTESIAN_POINT('Ctrl Pts',(81.3634179286217,22.0231789448313,-6.));
#13583=CARTESIAN_POINT('Ctrl Pts',(81.3581859277669,22.0340793373365,-6.));
#13584=CARTESIAN_POINT('Ctrl Pts',(81.3530615217638,22.045024878718,-6.));
#13585=CARTESIAN_POINT('Ctrl Pts',(81.3480477692262,22.0560102612827,-6.));
#13586=CARTESIAN_POINT('Ctrl Pts',(81.3195073639237,22.118543716704,-6.));
#13587=CARTESIAN_POINT('Ctrl Pts',(81.2945279303708,22.1824102238707,-6.));
#13588=CARTESIAN_POINT('Ctrl Pts',(81.2733329278551,22.2474053239885,-6.));
#13589=CARTESIAN_POINT('Ctrl Pts',(81.2541304646075,22.3062902436936,-6.));
#13590=CARTESIAN_POINT('Ctrl Pts',(81.2380346530873,22.3661021309141,-6.));
#13591=CARTESIAN_POINT('Ctrl Pts',(81.2252483675841,22.4266937631596,-6.));
#13592=CARTESIAN_POINT('Ctrl Pts',(81.2101158543187,22.4984036963139,-6.));
#13593=CARTESIAN_POINT('Ctrl Pts',(81.1996182649432,22.5712073072497,-6.));
#13594=CARTESIAN_POINT('Ctrl Pts',(81.1936804617054,22.6446815009142,-6.));
#13595=CARTESIAN_POINT('Ctrl Pts',(81.1923736340422,22.6608521460106,-6.));
#13596=CARTESIAN_POINT('Ctrl Pts',(81.1912878965242,22.677055190926,-6.));
#13597=CARTESIAN_POINT('Ctrl Pts',(81.1904228174184,22.693285960862,-6.));
#13598=CARTESIAN_POINT('Ctrl Pts',(81.1895274843029,22.7100843619741,-6.));
#13599=CARTESIAN_POINT('Ctrl Pts',(81.1888685034739,22.7269186557325,-6.));
#13600=CARTESIAN_POINT('Ctrl Pts',(81.1884459572869,22.7437493851286,-6.));
#13601=CARTESIAN_POINT('Ctrl Pts',(81.1867246939672,22.8123102147938,-6.));
#13602=CARTESIAN_POINT('Ctrl Pts',(81.1889150327053,22.8808986006225,-6.));
#13603=CARTESIAN_POINT('Ctrl Pts',(81.1948963902804,22.949176222518,-6.));
#13604=CARTESIAN_POINT('Ctrl Pts',(81.2008765126244,23.0174397441624,-6.));
#13605=CARTESIAN_POINT('Ctrl Pts',(81.2106465418321,23.0853937017974,-6.));
#13606=CARTESIAN_POINT('Ctrl Pts',(81.224135574421,23.1526849517223,-6.));
#13607=CARTESIAN_POINT('Ctrl Pts',(81.2338955665321,23.2013735484834,-6.));
#13608=CARTESIAN_POINT('Ctrl Pts',(81.2456035994461,23.2497149357491,-6.));
#13609=CARTESIAN_POINT('Ctrl Pts',(81.2592470183253,23.2975656941601,-6.));
#13610=CARTESIAN_POINT('Ctrl Pts',(81.2694833810369,23.3334670854062,-6.));
#13611=CARTESIAN_POINT('Ctrl Pts',(81.2808094559637,23.3690921381008,-6.));
#13612=CARTESIAN_POINT('Ctrl Pts',(81.2932238134428,23.4043761033473,-6.));
#13613=CARTESIAN_POINT('Ctrl Pts',(81.2973533007872,23.4161128918351,-6.));
#13614=CARTESIAN_POINT('Ctrl Pts',(81.3016000099352,23.427802745736,-6.));
#13615=CARTESIAN_POINT('Ctrl Pts',(81.3059632962339,23.43944310507,-6.));
#13616=CARTESIAN_POINT('Ctrl Pts',(81.3290872371389,23.5011330705975,-6.));
#13617=CARTESIAN_POINT('Ctrl Pts',(81.3554837692749,23.5614395006295,-6.));
#13618=CARTESIAN_POINT('Ctrl Pts',(81.3851028988208,23.6200283078873,-6.));
#13619=CARTESIAN_POINT('Ctrl Pts',(81.4059352451487,23.6612362144815,-6.));
#13620=CARTESIAN_POINT('Ctrl Pts',(81.4283626281757,23.7015939037268,-6.));
#13621=CARTESIAN_POINT('Ctrl Pts',(81.4523780545027,23.7409737879001,-6.));
#13622=CARTESIAN_POINT('Ctrl Pts',(81.460091064182,23.7536213846433,-6.));
#13623=CARTESIAN_POINT('Ctrl Pts',(81.4679690370099,23.7661697278492,-6.));
#13624=CARTESIAN_POINT('Ctrl Pts',(81.47600841658,23.7786089555933,-6.));
#13625=CARTESIAN_POINT('Ctrl Pts',(81.5102529542987,23.8315950846794,-6.));
#13626=CARTESIAN_POINT('Ctrl Pts',(81.5473532629023,23.8824974296264,-6.));
#13627=CARTESIAN_POINT('Ctrl Pts',(81.5872751057864,23.9310007715343,-6.));
#13628=CARTESIAN_POINT('Ctrl Pts',(81.6240617784761,23.9756950149413,-6.));
#13629=CARTESIAN_POINT('Ctrl Pts',(81.6632448080286,24.0183523539651,-6.));
#13630=CARTESIAN_POINT('Ctrl Pts',(81.7048188461966,24.0586932599642,-6.));
#13631=CARTESIAN_POINT('Ctrl Pts',(81.7126371936145,24.06627970651,-6.));
#13632=CARTESIAN_POINT('Ctrl Pts',(81.7205401543986,24.0737841268858,-6.));
#13633=CARTESIAN_POINT('Ctrl Pts',(81.7285261364169,24.0812058551231,-6.));
#13634=CARTESIAN_POINT('Origin',(83.,23.,-12.));
#13635=CARTESIAN_POINT('Origin',(83.,-23.,-18.));
#13636=CARTESIAN_POINT('Origin',(83.,23.,-18.));
#13637=CARTESIAN_POINT('Origin',(83.,-12.,-65.));
#13638=CARTESIAN_POINT('',(83.,-10.,-67.));
#13639=CARTESIAN_POINT('Origin',(83.,-10.,-65.));
#13640=CARTESIAN_POINT('',(83.,-14.,-67.));
#13641=CARTESIAN_POINT('',(83.,-12.,-67.));
#13642=CARTESIAN_POINT('Origin',(83.,-14.,-65.));
#13643=CARTESIAN_POINT('Origin',(83.,-2.22044604925031E-15,-40.));
#13644=CARTESIAN_POINT('',(83.,-10.,-44.));
#13645=CARTESIAN_POINT('Origin',(83.,-10.,-40.));
#13646=CARTESIAN_POINT('',(83.,-14.,-44.));
#13647=CARTESIAN_POINT('',(83.,-2.22044604925031E-15,-44.));
#13648=CARTESIAN_POINT('Origin',(83.,-14.,-40.));
#13649=CARTESIAN_POINT('Origin',(83.,-2.22044604925031E-15,-40.));
#13650=CARTESIAN_POINT('',(83.,14.,-44.));
#13651=CARTESIAN_POINT('Origin',(83.,14.,-40.));
#13652=CARTESIAN_POINT('',(83.,10.,-44.));
#13653=CARTESIAN_POINT('',(83.,-2.22044604925031E-15,-44.));
#13654=CARTESIAN_POINT('Origin',(83.,10.,-40.));
#13655=CARTESIAN_POINT('Origin',(77.,-10.,-70.));
#13656=CARTESIAN_POINT('',(77.,-10.,-50.));
#13657=CARTESIAN_POINT('',(77.,-14.,-50.));
#13658=CARTESIAN_POINT('',(77.,-11.,-50.));
#13659=CARTESIAN_POINT('',(77.,-10.,-70.));
#13660=CARTESIAN_POINT('',(77.,-10.,-70.));
#13661=CARTESIAN_POINT('',(77.,-14.,-70.));
#13662=CARTESIAN_POINT('',(77.,-10.,-70.));
#13663=CARTESIAN_POINT('',(77.,-14.,-70.));
#13664=CARTESIAN_POINT('Origin',(89.,-14.,-70.));
#13665=CARTESIAN_POINT('',(89.,-14.,-50.));
#13666=CARTESIAN_POINT('',(89.,-10.,-50.));
#13667=CARTESIAN_POINT('',(89.,-13.,-50.));
#13668=CARTESIAN_POINT('',(89.,-14.,-70.));
#13669=CARTESIAN_POINT('',(89.,-14.,-70.));
#13670=CARTESIAN_POINT('',(89.,-10.,-70.));
#13671=CARTESIAN_POINT('',(89.,-14.,-70.));
#13672=CARTESIAN_POINT('',(89.,-10.,-70.));
#13673=CARTESIAN_POINT('Origin',(83.,-12.,-70.));
#13674=CARTESIAN_POINT('',(89.,-10.,-70.));
#13675=CARTESIAN_POINT('',(77.,-14.,-70.));
#13676=CARTESIAN_POINT('Origin',(83.,-12.,-50.));
#13677=CARTESIAN_POINT('',(75.,-14.,-50.));
#13678=CARTESIAN_POINT('',(75.,-14.,-50.));
#13679=CARTESIAN_POINT('',(75.,-10.,-50.));
#13680=CARTESIAN_POINT('',(75.,-10.,-50.));
#13681=CARTESIAN_POINT('',(91.,-10.,-50.));
#13682=CARTESIAN_POINT('Origin',(83.,-12.,-50.));
#13683=CARTESIAN_POINT('',(91.,-10.,-50.));
#13684=CARTESIAN_POINT('',(91.,-10.,-50.));
#13685=CARTESIAN_POINT('',(91.,-14.,-50.));
#13686=CARTESIAN_POINT('',(91.,-14.,-50.));
#13687=CARTESIAN_POINT('',(75.,-14.,-50.));
#13688=CARTESIAN_POINT('Origin',(75.,10.,-50.));
#13689=CARTESIAN_POINT('',(75.,10.,-26.));
#13690=CARTESIAN_POINT('',(91.,10.,-26.));
#13691=CARTESIAN_POINT('',(79.,10.,-26.));
#13692=CARTESIAN_POINT('',(75.,10.,-50.));
#13693=CARTESIAN_POINT('',(75.,10.,-50.));
#13694=CARTESIAN_POINT('',(91.,10.,-50.));
#13695=CARTESIAN_POINT('',(75.,10.,-50.));
#13696=CARTESIAN_POINT('',(91.,10.,-50.));
#13697=CARTESIAN_POINT('Origin',(75.,14.,-50.));
#13698=CARTESIAN_POINT('',(75.,14.,-26.));
#13699=CARTESIAN_POINT('',(75.,7.,-26.));
#13700=CARTESIAN_POINT('',(75.,14.,-50.));
#13701=CARTESIAN_POINT('',(75.,14.,-50.));
#13702=CARTESIAN_POINT('',(75.,14.,-50.));
#13703=CARTESIAN_POINT('Origin',(91.,10.,-50.));
#13704=CARTESIAN_POINT('',(91.,14.,-26.));
#13705=CARTESIAN_POINT('',(91.,5.,-26.));
#13706=CARTESIAN_POINT('',(91.,14.,-50.));
#13707=CARTESIAN_POINT('',(91.,10.,-50.));
#13708=CARTESIAN_POINT('',(91.,14.,-50.));
#13709=CARTESIAN_POINT('Origin',(83.,12.,-50.));
#13710=CARTESIAN_POINT('',(91.,14.,-50.));
#13711=CARTESIAN_POINT('Origin',(83.,0.,-26.));
#13712=CARTESIAN_POINT('',(113.,14.,-26.));
#13713=CARTESIAN_POINT('',(113.,14.,-26.));
#13714=CARTESIAN_POINT('',(113.,-14.,-26.));
#13715=CARTESIAN_POINT('',(113.,-14.,-26.));
#13716=CARTESIAN_POINT('',(91.,-14.,-26.));
#13717=CARTESIAN_POINT('',(53.,-14.,-26.));
#13718=CARTESIAN_POINT('',(91.,-10.,-26.));
#13719=CARTESIAN_POINT('',(91.,-7.,-26.));
#13720=CARTESIAN_POINT('',(75.,-10.,-26.));
#13721=CARTESIAN_POINT('',(87.,-10.,-26.));
#13722=CARTESIAN_POINT('',(75.,-14.,-26.));
#13723=CARTESIAN_POINT('',(75.,-5.,-26.));
#13724=CARTESIAN_POINT('',(53.,-14.,-26.));
#13725=CARTESIAN_POINT('',(53.,-14.,-26.));
#13726=CARTESIAN_POINT('',(53.,14.,-26.));
#13727=CARTESIAN_POINT('',(53.,14.,-26.));
#13728=CARTESIAN_POINT('',(113.,14.,-26.));
#13729=CARTESIAN_POINT('',(94.,-4.,-26.));
#13730=CARTESIAN_POINT('',(102.,-4.,-26.));
#13731=CARTESIAN_POINT('',(92.5,-4.,-26.));
#13732=CARTESIAN_POINT('',(102.,4.,-26.));
#13733=CARTESIAN_POINT('',(102.,2.,-26.));
#13734=CARTESIAN_POINT('',(94.,4.,-26.));
#13735=CARTESIAN_POINT('',(88.5,4.,-26.));
#13736=CARTESIAN_POINT('',(94.,-2.,-26.));
#13737=CARTESIAN_POINT('',(64.,-4.,-26.));
#13738=CARTESIAN_POINT('',(72.,-4.,-26.));
#13739=CARTESIAN_POINT('',(77.5,-4.,-26.));
#13740=CARTESIAN_POINT('',(72.,4.,-26.));
#13741=CARTESIAN_POINT('',(72.,2.,-26.));
#13742=CARTESIAN_POINT('',(64.,4.,-26.));
#13743=CARTESIAN_POINT('',(73.5,4.,-26.));
#13744=CARTESIAN_POINT('',(64.,-2.,-26.));
#13745=CARTESIAN_POINT('Origin',(91.,-10.,-50.));
#13746=CARTESIAN_POINT('',(75.,-10.,-50.));
#13747=CARTESIAN_POINT('',(91.,-10.,-50.));
#13748=CARTESIAN_POINT('Origin',(91.,-14.,-50.));
#13749=CARTESIAN_POINT('',(91.,-14.,-50.));
#13750=CARTESIAN_POINT('Origin',(75.,-10.,-50.));
#13751=CARTESIAN_POINT('',(75.,-14.,-50.));
#13752=CARTESIAN_POINT('Origin',(53.,-14.,-26.));
#13753=CARTESIAN_POINT('',(113.,-14.,-12.));
#13754=CARTESIAN_POINT('',(113.,-14.,-26.));
#13755=CARTESIAN_POINT('',(88.,-14.,-12.));
#13756=CARTESIAN_POINT('',(53.,-14.,-12.));
#13757=CARTESIAN_POINT('',(88.,-14.,-20.));
#13758=CARTESIAN_POINT('',(88.,-14.,-23.));
#13759=CARTESIAN_POINT('',(78.,-14.,-20.));
#13760=CARTESIAN_POINT('',(68.,-14.,-20.));
#13761=CARTESIAN_POINT('',(78.,-14.,-12.));
#13762=CARTESIAN_POINT('',(78.,-14.,-23.));
#13763=CARTESIAN_POINT('',(53.,-14.,-12.));
#13764=CARTESIAN_POINT('',(53.,-14.,-12.));
#13765=CARTESIAN_POINT('',(53.,-14.,-26.));
#13766=CARTESIAN_POINT('Origin',(72.,-4.,-12.));
#13767=CARTESIAN_POINT('',(72.,-4.,-12.));
#13768=CARTESIAN_POINT('',(64.,-4.,-12.));
#13769=CARTESIAN_POINT('',(77.5,-4.,-12.));
#13770=CARTESIAN_POINT('',(72.,-4.,-12.));
#13771=CARTESIAN_POINT('',(64.,-4.,-12.));
#13772=CARTESIAN_POINT('Origin',(72.,4.,-12.));
#13773=CARTESIAN_POINT('',(72.,4.,-12.));
#13774=CARTESIAN_POINT('',(72.,2.,-12.));
#13775=CARTESIAN_POINT('',(72.,4.,-12.));
#13776=CARTESIAN_POINT('Origin',(64.,4.,-12.));
#13777=CARTESIAN_POINT('',(64.,4.,-12.));
#13778=CARTESIAN_POINT('',(73.5,4.,-12.));
#13779=CARTESIAN_POINT('',(64.,4.,-12.));
#13780=CARTESIAN_POINT('Origin',(64.,-4.,-12.));
#13781=CARTESIAN_POINT('',(64.,-2.,-12.));
#13782=CARTESIAN_POINT('Origin',(102.,-4.,-12.));
#13783=CARTESIAN_POINT('',(102.,-4.,-12.));
#13784=CARTESIAN_POINT('',(94.,-4.,-12.));
#13785=CARTESIAN_POINT('',(92.5,-4.,-12.));
#13786=CARTESIAN_POINT('',(102.,-4.,-12.));
#13787=CARTESIAN_POINT('',(94.,-4.,-12.));
#13788=CARTESIAN_POINT('Origin',(102.,4.,-12.));
#13789=CARTESIAN_POINT('',(102.,4.,-12.));
#13790=CARTESIAN_POINT('',(102.,2.,-12.));
#13791=CARTESIAN_POINT('',(102.,4.,-12.));
#13792=CARTESIAN_POINT('Origin',(94.,4.,-12.));
#13793=CARTESIAN_POINT('',(94.,4.,-12.));
#13794=CARTESIAN_POINT('',(88.5,4.,-12.));
#13795=CARTESIAN_POINT('',(94.,4.,-12.));
#13796=CARTESIAN_POINT('Origin',(94.,-4.,-12.));
#13797=CARTESIAN_POINT('',(94.,-2.,-12.));
#13798=CARTESIAN_POINT('Origin',(78.,30.,-20.));
#13799=CARTESIAN_POINT('',(78.,14.,-12.));
#13800=CARTESIAN_POINT('',(78.,14.,-20.));
#13801=CARTESIAN_POINT('',(78.,14.,-23.));
#13802=CARTESIAN_POINT('',(78.,15.,-12.));
#13803=CARTESIAN_POINT('',(78.,-30.,-20.));
#13804=CARTESIAN_POINT('',(78.,30.,-20.));
#13805=CARTESIAN_POINT('',(78.,-30.,-6.));
#13806=CARTESIAN_POINT('',(78.,-30.,-20.));
#13807=CARTESIAN_POINT('',(78.,30.,-6.));
#13808=CARTESIAN_POINT('',(78.,30.,-6.));
#13809=CARTESIAN_POINT('',(78.,30.,-20.));
#13810=CARTESIAN_POINT('',(78.,30.,-20.));
#13811=CARTESIAN_POINT('',(78.,30.,-20.));
#13812=CARTESIAN_POINT('Origin',(83.,0.,-20.));
#13813=CARTESIAN_POINT('',(88.,-30.,-20.));
#13814=CARTESIAN_POINT('',(88.,-30.,-20.));
#13815=CARTESIAN_POINT('',(78.,-30.,-20.));
#13816=CARTESIAN_POINT('Origin',(83.,0.,-20.));
#13817=CARTESIAN_POINT('',(88.,14.,-20.));
#13818=CARTESIAN_POINT('',(98.,14.,-20.));
#13819=CARTESIAN_POINT('',(88.,30.,-20.));
#13820=CARTESIAN_POINT('',(88.,30.,-20.));
#13821=CARTESIAN_POINT('',(88.,-30.,-20.));
#13822=CARTESIAN_POINT('Origin',(88.,30.,-20.));
#13823=CARTESIAN_POINT('',(88.,30.,-6.));
#13824=CARTESIAN_POINT('',(88.,30.,-6.));
#13825=CARTESIAN_POINT('',(88.,30.,-20.));
#13826=CARTESIAN_POINT('Origin',(88.,-30.,-20.));
#13827=CARTESIAN_POINT('',(88.,14.,-12.));
#13828=CARTESIAN_POINT('',(88.,14.,-23.));
#13829=CARTESIAN_POINT('',(88.,-30.,-6.));
#13830=CARTESIAN_POINT('',(88.,-30.,-6.));
#13831=CARTESIAN_POINT('',(88.,-30.,-20.));
#13832=CARTESIAN_POINT('',(88.,-15.,-12.));
#13833=CARTESIAN_POINT('Origin',(78.,-30.,-20.));
#13834=CARTESIAN_POINT('',(78.,-30.,-6.));
#13835=CARTESIAN_POINT('Origin',(83.,0.,-6.));
#13836=CARTESIAN_POINT('Origin',(83.,0.,-12.));
#13837=CARTESIAN_POINT('',(53.,14.,-12.));
#13838=CARTESIAN_POINT('',(113.,14.,-12.));
#13839=CARTESIAN_POINT('',(53.,14.,-12.));
#13840=CARTESIAN_POINT('Origin',(83.,0.,-12.));
#13841=CARTESIAN_POINT('',(113.,14.,-12.));
#13842=CARTESIAN_POINT('',(113.,-14.,-12.));
#13843=CARTESIAN_POINT('',(113.,14.,-12.));
#13844=CARTESIAN_POINT('Origin',(113.,14.,-26.));
#13845=CARTESIAN_POINT('',(53.,14.,-26.));
#13846=CARTESIAN_POINT('',(113.,14.,-26.));
#13847=CARTESIAN_POINT('Origin',(113.,-14.,-26.));
#13848=CARTESIAN_POINT('Origin',(53.,14.,-26.));
#13849=CARTESIAN_POINT('',(0.,0.,0.));
#13850=CARTESIAN_POINT('Origin',(0.,50.,5.));
#13851=CARTESIAN_POINT('',(-2.51343913234902,50.0006110695374,0.387416697508021));
#13852=CARTESIAN_POINT('',(-2.51566539374153,49.9965492175946,0.112583302491982));
#13853=CARTESIAN_POINT('',(-2.5175,50.,5.));
#13854=CARTESIAN_POINT('',(-1.91346599666504,51.635987203375,0.));
#13855=CARTESIAN_POINT('Ctrl Pts',(-2.51566539374153,49.9965492175946,0.112583302491982));
#13856=CARTESIAN_POINT('Ctrl Pts',(-2.51039880334568,50.5891289186517,0.0750555349946544));
#13857=CARTESIAN_POINT('Ctrl Pts',(-2.29922182808404,51.1848035603044,0.0375277674973273));
#13858=CARTESIAN_POINT('Ctrl Pts',(-1.91346599666504,51.635987203375,0.));
#13859=CARTESIAN_POINT('',(1.91709598686657,51.6387689967411,1.61160490543685E-15));
#13860=CARTESIAN_POINT('Origin',(0.,50.,0.));
#13861=CARTESIAN_POINT('Ctrl Pts',(1.91709858156531,51.6387709851531,1.07542748506512E-15));
#13862=CARTESIAN_POINT('Ctrl Pts',(1.38628707679971,52.2578898930047,0.0517824693358739));
#13863=CARTESIAN_POINT('Ctrl Pts',(0.526694557934675,52.5973407510515,0.103564938671746));
#13864=CARTESIAN_POINT('Ctrl Pts',(-0.283636619336389,52.50549272868,0.155347408007619));
#13865=CARTESIAN_POINT('Ctrl Pts',(-1.11189767700716,52.4116124211116,0.208275647749513));
#13866=CARTESIAN_POINT('Ctrl Pts',(-1.88869330258108,51.8671357122805,0.261203887491408));
#13867=CARTESIAN_POINT('Ctrl Pts',(-2.2589562141896,51.1206233620097,0.314132127233303));
#13868=CARTESIAN_POINT('Ctrl Pts',(-2.42984519203468,50.7760824196498,0.338560317324876));
#13869=CARTESIAN_POINT('Ctrl Pts',(-2.51413710353789,50.3885051034776,0.362988507416448));
#13870=CARTESIAN_POINT('Ctrl Pts',(-2.51343913234902,50.0006110695374,0.387416697508021));
#13871=CARTESIAN_POINT('Origin',(0.,50.,5.));
#13872=CARTESIAN_POINT('',(-2.51733703324273,49.9976965409071,1.38741669750802));
#13873=CARTESIAN_POINT('',(-2.52165773822405,50.0001226503677,1.11258330249199));
#13874=CARTESIAN_POINT('',(-2.5175,50.,5.));
#13875=CARTESIAN_POINT('Ctrl Pts',(-2.52165773822405,50.0001226503677,1.11258330249199));
#13876=CARTESIAN_POINT('Ctrl Pts',(-2.52166128694809,50.005845022657,1.11221987985459));
#13877=CARTESIAN_POINT('Ctrl Pts',(-2.52164349662147,50.0115673701366,1.11185645721719));
#13878=CARTESIAN_POINT('Ctrl Pts',(-2.52160430081332,50.0172895688312,1.11149303457979));
#13879=CARTESIAN_POINT('Ctrl Pts',(-2.51589589160278,50.85066061727,1.05856479483789));
#13880=CARTESIAN_POINT('Ctrl Pts',(-2.05616647103081,51.6808758587515,1.005636555096));
#13881=CARTESIAN_POINT('Ctrl Pts',(-1.35284854651385,52.1280190247019,0.952708315354104));
#13882=CARTESIAN_POINT('Ctrl Pts',(-0.64953062199688,52.5751621906524,0.899780075612209));
#13883=CARTESIAN_POINT('Ctrl Pts',(0.297375806465088,52.6392332810719,0.846851835870316));
#13884=CARTESIAN_POINT('Ctrl Pts',(1.05442258508657,52.2906908988364,0.793923596128421));
#13885=CARTESIAN_POINT('Ctrl Pts',(1.81146936370803,51.9421485166009,0.740995356386527));
#13886=CARTESIAN_POINT('Ctrl Pts',(2.37865649248901,51.1809926617104,0.688067116644633));
#13887=CARTESIAN_POINT('Ctrl Pts',(2.49637754307185,50.3560583642436,0.635138876902739));
#13888=CARTESIAN_POINT('Ctrl Pts',(2.61409859365469,49.5311240667767,0.582210637160844));
#13889=CARTESIAN_POINT('Ctrl Pts',(2.28235356603936,48.6424113267335,0.529282397418948));
#13890=CARTESIAN_POINT('Ctrl Pts',(1.65296007195949,48.0958828038186,0.476354157677053));
#13891=CARTESIAN_POINT('Ctrl Pts',(1.02356657787963,47.5493542809037,0.423425917935159));
#13892=CARTESIAN_POINT('Ctrl Pts',(0.0965246173352477,47.345009975117,0.370497678193264));
#13893=CARTESIAN_POINT('Ctrl Pts',(-0.703763051564332,47.5780837468121,
0.31756943845137));
#13894=CARTESIAN_POINT('Ctrl Pts',(-1.50405072046391,47.8111575185072,0.264641198709475));
#13895=CARTESIAN_POINT('Ctrl Pts',(-2.17758409771868,48.4816493676841,0.21171295896758));
#13896=CARTESIAN_POINT('Ctrl Pts',(-2.41595304962114,49.2787722121955,0.158784719225686));
#13897=CARTESIAN_POINT('Ctrl Pts',(-2.48531100381804,49.51071017768,0.143384246981118));
#13898=CARTESIAN_POINT('Ctrl Pts',(-2.51782667283229,49.7533690913194,0.12798377473655));
#13899=CARTESIAN_POINT('Ctrl Pts',(-2.51566539374153,49.9965492175946,0.112583302491982));
#13900=CARTESIAN_POINT('Ctrl Pts',(-2.51343913234902,50.0006110695374,0.387416697508021));
#13901=CARTESIAN_POINT('Ctrl Pts',(-2.51262481849839,49.5480601771088,0.415916747158344));
#13902=CARTESIAN_POINT('Ctrl Pts',(-2.39612581621068,49.0950781816461,0.444416796808667));
#13903=CARTESIAN_POINT('Ctrl Pts',(-2.16649440645853,48.7095058462719,0.472916846458989));
#13904=CARTESIAN_POINT('Ctrl Pts',(-1.74003948947585,47.9934486725154,0.525845086200883));
#13905=CARTESIAN_POINT('Ctrl Pts',(-0.923399457867387,47.509882316713,0.578773325942776));
#13906=CARTESIAN_POINT('Ctrl Pts',(-0.0905132172451013,47.4799853381815,
0.63170156568467));
#13907=CARTESIAN_POINT('Ctrl Pts',(0.742373023377197,47.45008835965,0.684629805426564));
#13908=CARTESIAN_POINT('Ctrl Pts',(1.59150547301333,47.8738607583895,0.73755804516846));
#13909=CARTESIAN_POINT('Ctrl Pts',(2.06826581498737,48.5574101224076,0.790486284910355));
#13910=CARTESIAN_POINT('Ctrl Pts',(2.54502615696142,49.2409594864258,0.84341452465225));
#13911=CARTESIAN_POINT('Ctrl Pts',(2.64941439127338,50.1842858157225,0.896342764394143));
#13912=CARTESIAN_POINT('Ctrl Pts',(2.33361478103381,50.95554584747,0.949271004136037));
#13913=CARTESIAN_POINT('Ctrl Pts',(2.01781517079425,51.7268058792174,1.00219924387793));
#13914=CARTESIAN_POINT('Ctrl Pts',(1.28182771600316,52.3259996134155,1.05512748361983));
#13915=CARTESIAN_POINT('Ctrl Pts',(0.462561219916565,52.4788730216424,1.10805572336172));
#13916=CARTESIAN_POINT('Ctrl Pts',(-0.356705276170035,52.6317464298693,
1.16098396310362));
#13917=CARTESIAN_POINT('Ctrl Pts',(-1.25925081355216,52.338299512125,1.21391220284551));
#13918=CARTESIAN_POINT('Ctrl Pts',(-1.83195103174541,51.7328440723438,1.26684044258741));
#13919=CARTESIAN_POINT('Ctrl Pts',(-2.26684204543177,51.2730797461156,1.30703252756094));
#13920=CARTESIAN_POINT('Ctrl Pts',(-2.51153043874408,50.6333982435079,1.34722461253448));
#13921=CARTESIAN_POINT('Ctrl Pts',(-2.51733703324273,49.9976965409071,1.38741669750802));
#13922=CARTESIAN_POINT('Origin',(0.,50.,5.));
#13923=CARTESIAN_POINT('',(-2.52130183071094,50.0008653446746,2.38741669750802));
#13924=CARTESIAN_POINT('',(-2.51579666705823,50.0021291253541,2.11258330249198));
#13925=CARTESIAN_POINT('',(-2.5175,50.,5.));
#13926=CARTESIAN_POINT('Ctrl Pts',(-2.51579666705823,50.0021291253541,2.11258330249198));
#13927=CARTESIAN_POINT('Ctrl Pts',(-2.51784694340528,50.257604699766,2.09645598497262));
#13928=CARTESIAN_POINT('Ctrl Pts',(-2.48205558212342,50.5125192663648,2.08032866745325));
#13929=CARTESIAN_POINT('Ctrl Pts',(-2.40604315257227,50.7548157476474,2.06420134993389));
#13930=CARTESIAN_POINT('Ctrl Pts',(-2.15657797711353,51.5500085151083,2.011273110192));
#13931=CARTESIAN_POINT('Ctrl Pts',(-1.47389705953297,52.2092935747538,1.9583448704501));
#13932=CARTESIAN_POINT('Ctrl Pts',(-0.67049187024376,52.4308904409638,1.9054166307082));
#13933=CARTESIAN_POINT('Ctrl Pts',(0.132913319045451,52.6524873071738,1.85248839096631));
#13934=CARTESIAN_POINT('Ctrl Pts',(1.05704278004332,52.4363959799482,1.79956015122442));
#13935=CARTESIAN_POINT('Ctrl Pts',(1.67888372485688,51.8815269103202,1.74663191148252));
#13936=CARTESIAN_POINT('Ctrl Pts',(2.30072466967044,51.3266578406921,1.69370367174063));
#13937=CARTESIAN_POINT('Ctrl Pts',(2.62027709829971,50.4330110286616,1.64077543199873));
#13938=CARTESIAN_POINT('Ctrl Pts',(2.49126884240055,49.6096529788875,1.58784719225684));
#13939=CARTESIAN_POINT('Ctrl Pts',(2.36226058650139,48.7862949291135,1.53491895251495));
#13940=CARTESIAN_POINT('Ctrl Pts',(1.7846916460738,48.0332256415959,1.48199071277305));
#13941=CARTESIAN_POINT('Ctrl Pts',(1.02293880729862,47.6951424070907,1.42906247303116));
#13942=CARTESIAN_POINT('Ctrl Pts',(0.261185968523444,47.3570591725854,1.37613423328926));
#13943=CARTESIAN_POINT('Ctrl Pts',(-0.684750768599321,47.4339619910925,
1.32320599354737));
#13944=CARTESIAN_POINT('Ctrl Pts',(-1.38187543823614,47.8906768280442,1.27027775380547));
#13945=CARTESIAN_POINT('Ctrl Pts',(-2.07421342145999,48.3442557112708,1.21771293670098));
#13946=CARTESIAN_POINT('Ctrl Pts',(-2.52114445696114,49.1724486921844,1.16514811959648));
#13947=CARTESIAN_POINT('Ctrl Pts',(-2.52165773822405,50.0001226503677,1.11258330249199));
#13948=CARTESIAN_POINT('Ctrl Pts',(-2.51733703324273,49.9976965409071,1.38741669750802));
#13949=CARTESIAN_POINT('Ctrl Pts',(-2.51917703945939,49.7962540112111,1.40015285227638));
#13950=CARTESIAN_POINT('Ctrl Pts',(-2.49702989601834,49.5952111103643,1.41288900704473));
#13951=CARTESIAN_POINT('Ctrl Pts',(-2.44934665571188,49.4004193485444,1.42562516181309));
#13952=CARTESIAN_POINT('Ctrl Pts',(-2.25118716248072,48.5909140263443,1.47855340155498));
#13953=CARTESIAN_POINT('Ctrl Pts',(-1.61201327701402,47.8893673437622,1.53148164129688));
#13954=CARTESIAN_POINT('Ctrl Pts',(-0.824403714088269,47.6169036636344,
1.58440988103877));
#13955=CARTESIAN_POINT('Ctrl Pts',(-0.0367941511625192,47.3444399835067,
1.63733812078066));
#13956=CARTESIAN_POINT('Ctrl Pts',(0.899251089222284,47.5010593058334,1.69026636052256));
#13957=CARTESIAN_POINT('Ctrl Pts',(1.55526611555618,48.0150718634765,1.74319460026445));
#13958=CARTESIAN_POINT('Ctrl Pts',(2.21128114189008,48.5290844211196,1.79612284000635));
#13959=CARTESIAN_POINT('Ctrl Pts',(2.58726595417309,49.4004902140791,1.84905107974824));
#13960=CARTESIAN_POINT('Ctrl Pts',(2.5111160610797,50.230409713109,1.90197931949014));
#13961=CARTESIAN_POINT('Ctrl Pts',(2.43496616798631,51.0603292121388,1.95490755923203));
#13962=CARTESIAN_POINT('Ctrl Pts',(1.90668156951655,51.8487624172389,2.00783579897393));
#13963=CARTESIAN_POINT('Ctrl Pts',(1.16808045474115,52.2348109074211,2.06076403871582));
#13964=CARTESIAN_POINT('Ctrl Pts',(0.429479339965766,52.6208593976033,2.11369227845772));
#13965=CARTESIAN_POINT('Ctrl Pts',(-0.519438291115244,52.6045231728675,
2.16662051819961));
#13966=CARTESIAN_POINT('Ctrl Pts',(-1.24431337085575,52.1932798198687,2.21954875794151));
#13967=CARTESIAN_POINT('Ctrl Pts',(-1.96918845059626,51.78203646687,2.2724769976834));
#13968=CARTESIAN_POINT('Ctrl Pts',(-2.47002097899627,50.9758859856083,2.32540523742529));
#13969=CARTESIAN_POINT('Ctrl Pts',(-2.51755893192147,50.1438371940777,2.37833347716719));
#13970=CARTESIAN_POINT('Ctrl Pts',(-2.52027832269835,50.0962401548622,2.3813612172808));
#13971=CARTESIAN_POINT('Ctrl Pts',(-2.52151436629643,50.0485583668156,2.38438895739441));
#13972=CARTESIAN_POINT('Ctrl Pts',(-2.52130183071094,50.0008653446746,2.38741669750802));
#13973=CARTESIAN_POINT('Origin',(0.,50.,5.));
#13974=CARTESIAN_POINT('',(-2.51477537127748,50.0017637133429,3.38741669750802));
#13975=CARTESIAN_POINT('',(-2.51410548455075,49.9986698388504,3.11258330249199));
#13976=CARTESIAN_POINT('',(-2.5175,50.,5.));
#13977=CARTESIAN_POINT('Ctrl Pts',(-2.51410548455075,49.9986698388504,3.11258330249199));
#13978=CARTESIAN_POINT('Ctrl Pts',(-2.5116808105572,50.5047191991178,3.08069209009065));
#13979=CARTESIAN_POINT('Ctrl Pts',(-2.36361132718456,51.0120740142689,3.04880087768932));
#13980=CARTESIAN_POINT('Ctrl Pts',(-2.07960156886363,51.4262003567888,3.01690966528799));
#13981=CARTESIAN_POINT('Ctrl Pts',(-1.60824487071502,52.1135049993496,2.9639814255461));
#13982=CARTESIAN_POINT('Ctrl Pts',(-0.762449251371702,52.5440176887533,
2.9110531858042));
#13983=CARTESIAN_POINT('Ctrl Pts',(0.0706293316935971,52.5206748274805,
2.85812494606231));
#13984=CARTESIAN_POINT('Ctrl Pts',(0.90370791475889,52.4973319662077,2.80519670632041));
#13985=CARTESIAN_POINT('Ctrl Pts',(1.72406946154617,52.0201335542584,2.75226846657852));
#13986=CARTESIAN_POINT('Ctrl Pts',(2.15620024718853,51.3075131635299,2.69934022683662));
#13987=CARTESIAN_POINT('Ctrl Pts',(2.5883310328309,50.5948927728014,2.64641198709473));
#13988=CARTESIAN_POINT('Ctrl Pts',(2.63223105732835,49.6468504032936,2.59348374735283));
#13989=CARTESIAN_POINT('Ctrl Pts',(2.26780545235797,48.8973447372696,2.54055550761094));
#13990=CARTESIAN_POINT('Ctrl Pts',(1.90337984738758,48.1478390712456,2.48762726786904));
#13991=CARTESIAN_POINT('Ctrl Pts',(1.13062861294936,47.5968701087052,2.43469902812715));
#13992=CARTESIAN_POINT('Ctrl Pts',(0.303272233527588,47.4966391080133,2.38177078838526));
#13993=CARTESIAN_POINT('Ctrl Pts',(-0.524084145894187,47.3964081073213,
2.32884254864336));
#13994=CARTESIAN_POINT('Ctrl Pts',(-1.40604567029951,47.7469150684777,2.27591430890147));
#13995=CARTESIAN_POINT('Ctrl Pts',(-1.93890171583371,48.387718786694,2.22298606915957));
#13996=CARTESIAN_POINT('Ctrl Pts',(-2.30939568999827,48.8332686086602,2.18618514693704));
#13997=CARTESIAN_POINT('Ctrl Pts',(-2.51111814192273,49.4191594695261,2.14938422471451));
#13998=CARTESIAN_POINT('Ctrl Pts',(-2.51579666705823,50.0021291253541,2.11258330249198));
#13999=CARTESIAN_POINT('Ctrl Pts',(-2.52130183071094,50.0008653446746,2.38741669750802));
#14000=CARTESIAN_POINT('Ctrl Pts',(-2.5177990096276,49.2148316877844,2.43731719713631));
#14001=CARTESIAN_POINT('Ctrl Pts',(-2.12082327730247,48.4257465499517,2.48721769676459));
#14002=CARTESIAN_POINT('Ctrl Pts',(-1.48602084271957,47.9627140408783,2.53711819639287));
#14003=CARTESIAN_POINT('Ctrl Pts',(-0.812701423142097,47.4715867810093,
2.59004643613477));
#14004=CARTESIAN_POINT('Ctrl Pts',(0.128180793463234,47.347279363071,2.64297467587666));
#14005=CARTESIAN_POINT('Ctrl Pts',(0.905944761878115,47.6466925048363,2.69590291561856));
#14006=CARTESIAN_POINT('Ctrl Pts',(1.683708730293,47.9461056466016,2.74883115536045));
#14007=CARTESIAN_POINT('Ctrl Pts',(2.29835445051743,48.6692393480704,2.80175939510235));
#14008=CARTESIAN_POINT('Ctrl Pts',(2.46853291167733,49.4850851180826,2.85468763484424));
#14009=CARTESIAN_POINT('Ctrl Pts',(2.63871137283723,50.3009308880947,2.90761587458614));
#14010=CARTESIAN_POINT('Ctrl Pts',(2.36442257493259,51.2094887266502,2.96054411432803));
#14011=CARTESIAN_POINT('Ctrl Pts',(1.77121995432369,51.7948737935868,3.01347235406992));
#14012=CARTESIAN_POINT('Ctrl Pts',(1.17801733371478,52.3802588605235,3.06640059381182));
#14013=CARTESIAN_POINT('Ctrl Pts',(0.265900890401605,52.6424711558412,3.11932883355372));
#14014=CARTESIAN_POINT('Ctrl Pts',(-0.547615609742164,52.461485164032,3.17225707329561));
#14015=CARTESIAN_POINT('Ctrl Pts',(-1.36113210988593,52.2804991722228,3.2251853130375));
#14016=CARTESIAN_POINT('Ctrl Pts',(-2.07604866686029,51.6563148932866,3.2781135527794));
#14017=CARTESIAN_POINT('Ctrl Pts',(-2.36511813044588,50.8746475269621,3.33104179252129));
#14018=CARTESIAN_POINT('Ctrl Pts',(-2.46774931324276,50.597124452181,3.34983342751687));
#14019=CARTESIAN_POINT('Ctrl Pts',(-2.51670106273314,50.2997501138417,3.36862506251244));
#14020=CARTESIAN_POINT('Ctrl Pts',(-2.51477537127748,50.0017637133429,3.38741669750802));
#14021=CARTESIAN_POINT('Origin',(0.,50.,5.));
#14022=CARTESIAN_POINT('',(-2.51492115541711,49.9981671707055,4.38741669750802));
#14023=CARTESIAN_POINT('',(-2.52064984019739,49.9985765242422,4.11258330249199));
#14024=CARTESIAN_POINT('',(-2.5175,50.,5.));
#14025=CARTESIAN_POINT('Ctrl Pts',(-2.52064984019739,49.9985765242422,4.11258330249199));
#14026=CARTESIAN_POINT('Ctrl Pts',(-2.51556776575615,50.7497542365495,4.06492819520869));
#14027=CARTESIAN_POINT('Ctrl Pts',(-2.15787617855472,51.5051323059894,4.01727308792539));
#14028=CARTESIAN_POINT('Ctrl Pts',(-1.57089146705521,51.9725846320086,3.96961798064209));
#14029=CARTESIAN_POINT('Ctrl Pts',(-0.918955729079003,52.4917614881716,
3.9166897409002));
#14030=CARTESIAN_POINT('Ctrl Pts',(0.0158240478079662,52.6557681645712,
3.8637615011583));
#14031=CARTESIAN_POINT('Ctrl Pts',(0.805560141658845,52.3895319602189,3.81083326141641));
#14032=CARTESIAN_POINT('Ctrl Pts',(1.59529623550971,52.1232957558667,3.75790502167451));
#14033=CARTESIAN_POINT('Ctrl Pts',(2.2399886463245,51.4268166707627,3.70497678193262));
#14034=CARTESIAN_POINT('Ctrl Pts',(2.44453474790488,50.6189022524807,3.65204854219073));
#14035=CARTESIAN_POINT('Ctrl Pts',(2.64908084948526,49.8109878341986,3.59912030244883));
#14036=CARTESIAN_POINT('Ctrl Pts',(2.41348064183123,48.8916380827385,3.54619206270694));
#14037=CARTESIAN_POINT('Ctrl Pts',(1.84557817412316,48.2816777553516,3.49326382296504));
#14038=CARTESIAN_POINT('Ctrl Pts',(1.27767570641509,47.6717174279646,3.44033558322315));
#14039=CARTESIAN_POINT('Ctrl Pts',(0.377470978652977,47.3711465246507,3.38740734348125));
#14040=CARTESIAN_POINT('Ctrl Pts',(-0.442974730529885,47.517548889903,3.33447910373936));
#14041=CARTESIAN_POINT('Ctrl Pts',(-1.26342043971276,47.6639512551553,3.28155086399746));
#14042=CARTESIAN_POINT('Ctrl Pts',(-2.00410713031638,48.2573268889739,3.22862262425557));
#14043=CARTESIAN_POINT('Ctrl Pts',(-2.32599158714125,49.0260630037421,3.17569438451367));
#14044=CARTESIAN_POINT('Ctrl Pts',(-2.4539288121793,49.3316073170032,3.15465735717311));
#14045=CARTESIAN_POINT('Ctrl Pts',(-2.51570491992036,49.6648545516281,3.13362032983255));
#14046=CARTESIAN_POINT('Ctrl Pts',(-2.51410548455075,49.9986698388504,3.11258330249199));
#14047=CARTESIAN_POINT('Ctrl Pts',(-2.51477537127748,50.0017637133429,3.38741669750802));
#14048=CARTESIAN_POINT('Ctrl Pts',(-2.51127718880957,49.4604460485417,3.42155330225434));
#14049=CARTESIAN_POINT('Ctrl Pts',(-2.33988439025294,48.917108589911,3.45568990700066));
#14050=CARTESIAN_POINT('Ctrl Pts',(-2.01739407194983,48.48708452822,3.48982651174697));
#14051=CARTESIAN_POINT('Ctrl Pts',(-1.51737817967137,47.8203393495149,3.54275475148887));
#14052=CARTESIAN_POINT('Ctrl Pts',(-0.654124024917635,47.4259994458174,
3.59568299123076));
#14053=CARTESIAN_POINT('Ctrl Pts',(0.177220933403488,47.4845706513577,3.64861123097266));
#14054=CARTESIAN_POINT('Ctrl Pts',(1.00856589172461,47.5431418568979,3.70153947071455));
#14055=CARTESIAN_POINT('Ctrl Pts',(1.80800165361312,48.0546241716759,3.75446771045645));
#14056=CARTESIAN_POINT('Ctrl Pts',(2.20959310192558,48.7848907905357,3.80739595019834));
#14057=CARTESIAN_POINT('Ctrl Pts',(2.61118455023805,49.5151574093954,3.86032418994024));
#14058=CARTESIAN_POINT('Ctrl Pts',(2.61493168497446,50.4642083323369,3.91325242968213));
#14059=CARTESIAN_POINT('Ctrl Pts',(2.2191192862364,51.1976233382602,3.96618066942402));
#14060=CARTESIAN_POINT('Ctrl Pts',(1.82330688749833,51.9310383441836,4.01910890916592));
#14061=CARTESIAN_POINT('Ctrl Pts',(1.02793495528578,52.4488174330888,4.07203714890781));
#14062=CARTESIAN_POINT('Ctrl Pts',(0.197078422081479,52.5139515036224,4.12496538864971));
#14063=CARTESIAN_POINT('Ctrl Pts',(-0.633778111122818,52.5790855741559,
4.1778936283916));
#14064=CARTESIAN_POINT('Ctrl Pts',(-1.50011924531886,52.1915746263178,4.2308218681335));
#14065=CARTESIAN_POINT('Ctrl Pts',(-2.00538448193382,51.5287985958244,4.28375010787539));
#14066=CARTESIAN_POINT('Ctrl Pts',(-2.33525957441895,51.0960886278467,4.31830563775293));
#14067=CARTESIAN_POINT('Ctrl Pts',(-2.51122754678017,50.5460480475906,4.35286116763048));
#14068=CARTESIAN_POINT('Ctrl Pts',(-2.51492115541711,49.9981671707055,4.38741669750802));
#14069=CARTESIAN_POINT('Origin',(0.,50.,5.));
#14070=CARTESIAN_POINT('',(-2.52139129543236,49.9992487982722,5.38741669750802));
#14071=CARTESIAN_POINT('',(-2.51841387510379,50.0022201728711,5.11258330249199));
#14072=CARTESIAN_POINT('',(-2.5175,50.,5.));
#14073=CARTESIAN_POINT('Ctrl Pts',(-2.51841387510379,50.0022201728711,5.11258330249199));
#14074=CARTESIAN_POINT('Ctrl Pts',(-2.51993725434446,50.167966042206,5.10209254006862));
#14075=CARTESIAN_POINT('Ctrl Pts',(-2.50497422321175,50.3334381998588,5.09160177764525));
#14076=CARTESIAN_POINT('Ctrl Pts',(-2.47252158136002,50.4954060568224,5.08111101522188));
#14077=CARTESIAN_POINT('Ctrl Pts',(-2.3087907542888,51.3125700738777,5.02818277547998));
#14078=CARTESIAN_POINT('Ctrl Pts',(-1.69987449903624,52.0405346440253,4.97525453573809));
#14079=CARTESIAN_POINT('Ctrl Pts',(-0.924499202043288,52.3460799979661,
4.92232629599619));
#14080=CARTESIAN_POINT('Ctrl Pts',(-0.149123905050339,52.651625351907,4.8693980562543));
#14081=CARTESIAN_POINT('Ctrl Pts',(0.792710433683001,52.5347514896411,4.8164698165124));
#14082=CARTESIAN_POINT('Ctrl Pts',(1.46988692476992,52.048956456299,4.76354157677051));
#14083=CARTESIAN_POINT('Ctrl Pts',(2.14706341585683,51.5631614229569,4.71061333702861));
#14084=CARTESIAN_POINT('Ctrl Pts',(2.55958205929732,50.7084452185386,4.65768509728672));
#14085=CARTESIAN_POINT('Ctrl Pts',(2.51861585329202,49.8760471259917,4.60475685754483));
#14086=CARTESIAN_POINT('Ctrl Pts',(2.47764964728673,49.0436490334448,4.55182861780293));
#14087=CARTESIAN_POINT('Ctrl Pts',(1.98319859183565,48.2335690527693,4.49890037806103));
#14088=CARTESIAN_POINT('Ctrl Pts',(1.26159357360843,47.8166146042215,4.44597213831914));
#14089=CARTESIAN_POINT('Ctrl Pts',(0.539988555381206,47.3996601556737,4.39304389857725));
#14090=CARTESIAN_POINT('Ctrl Pts',(-0.408770425622154,47.3758312392538,
4.34011565883535));
#14091=CARTESIAN_POINT('Ctrl Pts',(-1.1503967822133,47.7560353445703,4.28718741909346));
#14092=CARTESIAN_POINT('Ctrl Pts',(-1.89202313880445,48.1362394498869,4.23425917935156));
#14093=CARTESIAN_POINT('Ctrl Pts',(-2.42651687098339,48.9204765769399,4.18133093960967));
#14094=CARTESIAN_POINT('Ctrl Pts',(-2.50921788754013,49.7497686584296,4.12840269986777));
#14095=CARTESIAN_POINT('Ctrl Pts',(-2.51745722096386,49.832389335291,4.12312956740918));
#14096=CARTESIAN_POINT('Ctrl Pts',(-2.52121218184807,49.9154572154682,4.11785643495058));
#14097=CARTESIAN_POINT('Ctrl Pts',(-2.52064984019739,49.9985765242422,4.11258330249199));
#14098=CARTESIAN_POINT('Ctrl Pts',(-2.51492115541711,49.9981671707055,4.38741669750802));
#14099=CARTESIAN_POINT('Ctrl Pts',(-2.51688499738623,49.7068662869712,4.40578940737237));
#14100=CARTESIAN_POINT('Ctrl Pts',(-2.47014850145045,49.4161759310116,4.42416211723673));
#14101=CARTESIAN_POINT('Ctrl Pts',(-2.37195102004796,49.1440558280711,4.44253482710108));
#14102=CARTESIAN_POINT('Ctrl Pts',(-2.08906298251325,48.3601302039597,4.49546306684297));
#14103=CARTESIAN_POINT('Ctrl Pts',(-1.37909756840994,47.7303200688855,4.54839130658487));
#14104=CARTESIAN_POINT('Ctrl Pts',(-0.567035582013418,47.5429158102107,
4.60131954632676));
#14105=CARTESIAN_POINT('Ctrl Pts',(0.245026404383105,47.3555115515358,4.65424778606865));
#14106=CARTESIAN_POINT('Ctrl Pts',(1.15918496307284,47.6105131692602,4.70717602581055));
#14107=CARTESIAN_POINT('Ctrl Pts',(1.7569915643907,48.1911957790756,4.76010426555244));
#14108=CARTESIAN_POINT('Ctrl Pts',(2.35479816570856,48.771878388891,4.81303250529434));
#14109=CARTESIAN_POINT('Ctrl Pts',(2.63625280965454,49.6782419907974,4.86596074503623));
#14110=CARTESIAN_POINT('Ctrl Pts',(2.47252195766438,50.4954061322205,4.91888898477813));
#14111=CARTESIAN_POINT('Ctrl Pts',(2.30879110567422,51.3125702736437,4.97181722452002));
#14112=CARTESIAN_POINT('Ctrl Pts',(1.69987475774791,52.0405349545835,5.02474546426192));
#14113=CARTESIAN_POINT('Ctrl Pts',(0.924499342747056,52.3460803550268,5.07767370400381));
#14114=CARTESIAN_POINT('Ctrl Pts',(0.149123927746205,52.65162575547,5.13060194374571));
#14115=CARTESIAN_POINT('Ctrl Pts',(-0.792710554329193,52.5347518754165,
5.1835301834876));
#14116=CARTESIAN_POINT('Ctrl Pts',(-1.46988714847869,52.048956768139,5.23645842322949));
#14117=CARTESIAN_POINT('Ctrl Pts',(-2.11368593801667,51.5871063369063,5.286777847989));
#14118=CARTESIAN_POINT('Ctrl Pts',(-2.5182736560907,50.7918063994386,5.33709727274851));
#14119=CARTESIAN_POINT('Ctrl Pts',(-2.52139129543236,49.9992487982722,5.38741669750802));
#14120=CARTESIAN_POINT('Origin',(0.,50.,5.));
#14121=CARTESIAN_POINT('',(-2.51713805421624,50.0023011578997,6.38741669750802));
#14122=CARTESIAN_POINT('',(-2.51340291777706,50.0000546149131,6.11258330249199));
#14123=CARTESIAN_POINT('',(-2.5175,50.,5.));
#14124=CARTESIAN_POINT('Ctrl Pts',(-2.51340291777706,50.0000546149131,6.11258330249199));
#14125=CARTESIAN_POINT('Ctrl Pts',(-2.51348357000391,50.4169542413391,6.08632864518665));
#14126=CARTESIAN_POINT('Ctrl Pts',(-2.41545869747094,50.8338181852126,6.06007398788131));
#14127=CARTESIAN_POINT('Ctrl Pts',(-2.21911894849843,51.1976231559884,6.03381933057598));
#14128=CARTESIAN_POINT('Ctrl Pts',(-1.82330661000076,51.9310380502898,5.98089109083408));
#14129=CARTESIAN_POINT('Ctrl Pts',(-1.02793479883965,52.4488170603922,5.92796285109219));
#14130=CARTESIAN_POINT('Ctrl Pts',(-0.197078392087235,52.5139511210127,
5.87503461135029));
#14131=CARTESIAN_POINT('Ctrl Pts',(0.633778014665187,52.5790851816333,5.8221063716084));
#14132=CARTESIAN_POINT('Ctrl Pts',(1.50011901700892,52.191574292772,5.76917813186651));
#14133=CARTESIAN_POINT('Ctrl Pts',(2.00538417672529,51.5287983631495,5.71624989212461));
#14134=CARTESIAN_POINT('Ctrl Pts',(2.51064933644165,50.866022433527,5.66332165238272));
#14135=CARTESIAN_POINT('Ctrl Pts',(2.65483865353065,49.9279814631433,5.61039341264082));
#14136=CARTESIAN_POINT('Ctrl Pts',(2.37195065904994,49.1440559583411,5.55746517289893));
#14137=CARTESIAN_POINT('Ctrl Pts',(2.08906266456923,48.360130453539,5.50453693315704));
#14138=CARTESIAN_POINT('Ctrl Pts',(1.3790973585188,47.7303204143184,5.45160869341514));
#14139=CARTESIAN_POINT('Ctrl Pts',(0.567035495713689,47.5429161841654,5.39868045367324));
#14140=CARTESIAN_POINT('Ctrl Pts',(-0.245026367091423,47.3555119540124,
5.34575221393135));
#14141=CARTESIAN_POINT('Ctrl Pts',(-1.15918478665122,47.610513532927,5.29282397418945));
#14142=CARTESIAN_POINT('Ctrl Pts',(-1.75699129698618,48.1911960543657,5.23989573444756));
#14143=CARTESIAN_POINT('Ctrl Pts',(-2.23630820506625,48.6567830728078,5.19745825712904));
#14144=CARTESIAN_POINT('Ctrl Pts',(-2.5122514657989,49.3317411088454,5.15502077981051));
#14145=CARTESIAN_POINT('Ctrl Pts',(-2.51841387510379,50.0022201728711,5.11258330249199));
#14146=CARTESIAN_POINT('Ctrl Pts',(-2.52139129543236,49.9992487982722,5.38741669750802));
#14147=CARTESIAN_POINT('Ctrl Pts',(-2.521552929717,49.9581585800472,5.39002551249041));
#14148=CARTESIAN_POINT('Ctrl Pts',(-2.5206354473163,49.9170757329839,5.39263432747279));
#14149=CARTESIAN_POINT('Ctrl Pts',(-2.51861623661168,49.8760471071268,5.39524314245518));
#14150=CARTESIAN_POINT('Ctrl Pts',(-2.47765002437156,49.0436488878934,5.44817138219707));
#14151=CARTESIAN_POINT('Ctrl Pts',(-1.98319889366771,48.2335687839283,5.50109962193897));
#14152=CARTESIAN_POINT('Ctrl Pts',(-1.26159376561614,47.8166142719222,5.55402786168086));
#14153=CARTESIAN_POINT('Ctrl Pts',(-0.539988637564569,47.3996597599162,
5.60695610142275));
#14154=CARTESIAN_POINT('Ctrl Pts',(0.40877048783472,47.3758308398693,5.65988434116465));
#14155=CARTESIAN_POINT('Ctrl Pts',(1.15039695729739,47.7560350030509,5.71281258090654));
#14156=CARTESIAN_POINT('Ctrl Pts',(1.89202342676006,48.1362391662326,5.76574082064844));
#14157=CARTESIAN_POINT('Ctrl Pts',(2.42651724028611,48.9204764126428,5.81866906039033));
#14158=CARTESIAN_POINT('Ctrl Pts',(2.50921826942949,49.749768620346,5.87159730013223));
#14159=CARTESIAN_POINT('Ctrl Pts',(2.59191929857286,50.5790608280491,5.92452553987412));
#14160=CARTESIAN_POINT('Ctrl Pts',(2.22282754333358,51.4534079970451,5.97745377961602));
#14161=CARTESIAN_POINT('Ctrl Pts',(1.57089170613635,51.9725849322246,6.03038201935791));
#14162=CARTESIAN_POINT('Ctrl Pts',(0.918955868939124,52.4917618674041,6.08331025909981));
#14163=CARTESIAN_POINT('Ctrl Pts',(-0.0158240502160405,52.655768568767,
6.1362384988417));
#14164=CARTESIAN_POINT('Ctrl Pts',(-0.805560264260574,52.389532323894,6.18916673858359));
#14165=CARTESIAN_POINT('Ctrl Pts',(-1.59529647830511,52.1232960790209,6.24209497832549));
#14166=CARTESIAN_POINT('Ctrl Pts',(-2.23998898723901,51.4268168879119,6.29502321806738));
#14167=CARTESIAN_POINT('Ctrl Pts',(-2.44453511994999,50.6189023466718,6.34795145780928));
#14168=CARTESIAN_POINT('Ctrl Pts',(-2.49537415657931,50.418098760649,6.36110653770886));
#14169=CARTESIAN_POINT('Ctrl Pts',(-2.51902319308404,50.2104112665728,6.37426161760844));
#14170=CARTESIAN_POINT('Ctrl Pts',(-2.51713805421624,50.0023011578997,6.38741669750802));
#14171=CARTESIAN_POINT('Origin',(0.,50.,5.));
#14172=CARTESIAN_POINT('',(-2.51354891404356,49.9993677900347,7.38741669750802));
#14173=CARTESIAN_POINT('',(-2.51821333355664,49.9977519369613,7.11258330249199));
#14174=CARTESIAN_POINT('',(-2.5175,50.,5.));
#14175=CARTESIAN_POINT('Ctrl Pts',(-2.51821333355664,49.9977519369613,7.11258330249199));
#14176=CARTESIAN_POINT('Ctrl Pts',(-2.51208745167034,50.6617483076158,7.07056475030469));
#14177=CARTESIAN_POINT('Ctrl Pts',(-2.24214997829159,51.3301494078962,7.02854619811738));
#14178=CARTESIAN_POINT('Ctrl Pts',(-1.77121968474941,51.7948735204092,6.98652764593008));
#14179=CARTESIAN_POINT('Ctrl Pts',(-1.17801715441916,52.3802584982467,6.93359940618819));
#14180=CARTESIAN_POINT('Ctrl Pts',(-0.265900849933291,52.642470753672,6.88067116644629));
#14181=CARTESIAN_POINT('Ctrl Pts',(0.547615526395802,52.4614847894114,6.8277429267044));
#14182=CARTESIAN_POINT('Ctrl Pts',(1.36113190272489,52.2804988251508,6.7748146869625));
#14183=CARTESIAN_POINT('Ctrl Pts',(2.07604835089721,51.6563146412042,6.72188644722061));
#14184=CARTESIAN_POINT('Ctrl Pts',(2.36511777048901,50.8746473938434,6.66895820747871));
#14185=CARTESIAN_POINT('Ctrl Pts',(2.65418719008082,50.0929801464827,6.61602996773682));
#14186=CARTESIAN_POINT('Ctrl Pts',(2.51740958109211,49.1538298357076,6.56310172799492));
#14187=CARTESIAN_POINT('Ctrl Pts',(2.01739376491279,48.4870847584785,6.51017348825303));
#14188=CARTESIAN_POINT('Ctrl Pts',(1.51737794873347,47.8203396812494,6.45724524851113));
#14189=CARTESIAN_POINT('Ctrl Pts',(0.654123925363523,47.4259998375662,6.40431700876924));
#14190=CARTESIAN_POINT('Ctrl Pts',(-0.177220906431141,47.4845710341917,
6.35138876902734));
#14191=CARTESIAN_POINT('Ctrl Pts',(-1.00856573822581,47.5431422308173,6.29846052928545));
#14192=CARTESIAN_POINT('Ctrl Pts',(-1.80800137844519,48.0546244677515,6.24553228954355));
#14193=CARTESIAN_POINT('Ctrl Pts',(-2.20959276563777,48.784890975469,6.19260404980166));
#14194=CARTESIAN_POINT('Ctrl Pts',(-2.41197774999261,49.1529142460188,6.1659304673651));
#14195=CARTESIAN_POINT('Ctrl Pts',(-2.51332097864539,49.5765028456433,6.13925688492854));
#14196=CARTESIAN_POINT('Ctrl Pts',(-2.51340291777706,50.0000546149131,6.11258330249199));
#14197=CARTESIAN_POINT('Ctrl Pts',(-2.51713805421624,50.0023011578997,6.38741669750802));
#14198=CARTESIAN_POINT('Ctrl Pts',(-2.51143851228367,49.3730996114068,6.42718985735034));
#14199=CARTESIAN_POINT('Ctrl Pts',(-2.27233134100759,48.7400349493151,6.46696301719265));
#14200=CARTESIAN_POINT('Ctrl Pts',(-1.84557845500972,48.2816774938369,6.50673617703496));
#14201=CARTESIAN_POINT('Ctrl Pts',(-1.27767590087041,47.6717170736132,6.55966441677686));
#14202=CARTESIAN_POINT('Ctrl Pts',(-0.377471036103719,47.3711461245372,
6.61259265651875));
#14203=CARTESIAN_POINT('Ctrl Pts',(0.442974797947392,47.5175485120787,6.66552089626065));
#14204=CARTESIAN_POINT('Ctrl Pts',(1.2634206319985,47.6639508996202,6.71844913600254));
#14205=CARTESIAN_POINT('Ctrl Pts',(2.00410743533403,48.2573266237792,6.77137737574443));
#14206=CARTESIAN_POINT('Ctrl Pts',(2.32599194114623,49.0260628555307,6.82430561548633));
#14207=CARTESIAN_POINT('Ctrl Pts',(2.64787644695843,49.7947990872822,6.87723385522822));
#14208=CARTESIAN_POINT('Ctrl Pts',(2.55095865524729,50.7388958266262,6.93016209497012));
#14209=CARTESIAN_POINT('Ctrl Pts',(2.07960188536427,51.4262005738175,6.98309033471202));
#14210=CARTESIAN_POINT('Ctrl Pts',(1.60824511548125,52.1135053210088,7.03601857445391));
#14211=CARTESIAN_POINT('Ctrl Pts',(0.762449367426351,52.5440180760474,7.0889468141958));
#14212=CARTESIAN_POINT('Ctrl Pts',(-0.0706293424360422,52.5206752111724,
7.14187505393769));
#14213=CARTESIAN_POINT('Ctrl Pts',(-0.903708052298439,52.4973323462974,
7.19480329367959));
#14214=CARTESIAN_POINT('Ctrl Pts',(-1.72406972396833,52.0201338615088,7.24773153342148));
#14215=CARTESIAN_POINT('Ctrl Pts',(-2.15620057536443,51.3075133624157,7.30065977316338));
#14216=CARTESIAN_POINT('Ctrl Pts',(-2.39230858225818,50.9181511931355,7.32957874794493));
#14217=CARTESIAN_POINT('Ctrl Pts',(-2.512517267736,50.4585080201858,7.35849772272647));
#14218=CARTESIAN_POINT('Ctrl Pts',(-2.51354891404356,49.9993677900347,7.38741669750802));
#14219=CARTESIAN_POINT('Origin',(0.,50.,5.));
#14220=CARTESIAN_POINT('',(-2.51945660451951,49.9980217824357,8.38741669750802));
#14221=CARTESIAN_POINT('',(-2.52079116141582,50.0013273547755,8.11258330249199));
#14222=CARTESIAN_POINT('',(-2.5175,50.,5.));
#14223=CARTESIAN_POINT('Ctrl Pts',(-2.52079116141582,50.0013273547755,8.11258330249199));
#14224=CARTESIAN_POINT('Ctrl Pts',(-2.52128051842586,50.0778319453862,8.10772909516462));
#14225=CARTESIAN_POINT('Ctrl Pts',(-2.51809961281036,50.1542952883015,8.10287488783724));
#14226=CARTESIAN_POINT('Ctrl Pts',(-2.51111567921584,50.2304096787005,8.09802068050987));
#14227=CARTESIAN_POINT('Ctrl Pts',(-2.43496579794733,51.0603290519682,8.04509244076797));
#14228=CARTESIAN_POINT('Ctrl Pts',(-1.90668127928963,51.8487621358105,7.99216420102608));
#14229=CARTESIAN_POINT('Ctrl Pts',(-1.16808027679305,52.234810566944,7.93923596128418));
#14230=CARTESIAN_POINT('Ctrl Pts',(-0.429479274296469,52.6208589980775,
7.88630772154228));
#14231=CARTESIAN_POINT('Ctrl Pts',(0.519438212038995,52.6045227765023,7.83337948180039));
#14232=CARTESIAN_POINT('Ctrl Pts',(1.24431318138389,52.1932794862502,7.7804512420585));
#14233=CARTESIAN_POINT('Ctrl Pts',(1.96918815072878,51.782036195998,7.7275230023166));
#14234=CARTESIAN_POINT('Ctrl Pts',(2.47002060308309,50.975885837069,7.67459476257471));
#14235=CARTESIAN_POINT('Ctrl Pts',(2.51755854881386,50.1438371720874,7.62166652283282));
#14236=CARTESIAN_POINT('Ctrl Pts',(2.56509649454462,49.3117885071058,7.56873828309093));
#14237=CARTESIAN_POINT('Ctrl Pts',(2.15933993365185,48.4538415360717,7.51581004334903));
#14238=CARTESIAN_POINT('Ctrl Pts',(1.48602061652768,47.9627143509944,7.46288180360713));
#14239=CARTESIAN_POINT('Ctrl Pts',(0.812701299403498,47.4715871659172,7.40995356386523));
#14240=CARTESIAN_POINT('Ctrl Pts',(-0.128180773952088,47.3472797667968,
7.35702532412334));
#14241=CARTESIAN_POINT('Ctrl Pts',(-0.90594462398342,47.6466928629692,7.30409708438145));
#14242=CARTESIAN_POINT('Ctrl Pts',(-1.68370847401475,47.9461059591416,7.25116884463955));
#14243=CARTESIAN_POINT('Ctrl Pts',(-2.29835410072182,48.6692395506069,7.19824060489766));
#14244=CARTESIAN_POINT('Ctrl Pts',(-2.46853253598805,49.4850851964644,7.14531236515576));
#14245=CARTESIAN_POINT('Ctrl Pts',(-2.50361009697133,49.6532491318698,7.13440267760117));
#14246=CARTESIAN_POINT('Ctrl Pts',(-2.5198038561686,49.8253520668056,7.12349299004658));
#14247=CARTESIAN_POINT('Ctrl Pts',(-2.51821333355664,49.9977519369613,7.11258330249199));
#14248=CARTESIAN_POINT('Ctrl Pts',(-2.51354891404356,49.9993677900347,7.38741669750802));
#14249=CARTESIAN_POINT('Ctrl Pts',(-2.51440541292469,49.6181779476241,7.41142596246837));
#14250=CARTESIAN_POINT('Ctrl Pts',(-2.4331162684414,49.2373347706455,7.43543522742872));
#14251=CARTESIAN_POINT('Ctrl Pts',(-2.26780579747753,48.8973445696587,7.45944449238906));
#14252=CARTESIAN_POINT('Ctrl Pts',(-1.9033801370722,48.1478387893924,7.51237273213096));
#14253=CARTESIAN_POINT('Ctrl Pts',(-1.13062878513921,47.5968697422575,7.56530097187285));
#14254=CARTESIAN_POINT('Ctrl Pts',(-0.303272279740653,47.4966387266282,
7.61822921161475));
#14255=CARTESIAN_POINT('Ctrl Pts',(0.524084225657901,47.3964077109989,7.67115745135664));
#14256=CARTESIAN_POINT('Ctrl Pts',(1.40604588452202,47.7469147268753,7.72408569109854));
#14257=CARTESIAN_POINT('Ctrl Pts',(1.93890201103807,48.3877185420343,7.77701393084044));
#14258=CARTESIAN_POINT('Ctrl Pts',(2.47175813755411,49.0285223571934,7.82994217058233));
#14259=CARTESIAN_POINT('Ctrl Pts',(2.6555087317221,49.9596229716351,7.88287041032422));
#14260=CARTESIAN_POINT('Ctrl Pts',(2.40604351852937,50.7548158611892,7.93579865006612));
#14261=CARTESIAN_POINT('Ctrl Pts',(2.15657830533664,51.5500087507433,7.98872688980801));
#14262=CARTESIAN_POINT('Ctrl Pts',(1.4738972847832,52.2092939154097,8.0416551295499));
#14263=CARTESIAN_POINT('Ctrl Pts',(0.670491972751082,52.4308908134011,8.09458336929179));
#14264=CARTESIAN_POINT('Ctrl Pts',(-0.132913339281037,52.6524877113925,
8.14751160903369));
#14265=CARTESIAN_POINT('Ctrl Pts',(-1.05704294279184,52.4363963427089,8.20043984877559));
#14266=CARTESIAN_POINT('Ctrl Pts',(-1.67888398130339,51.881527192142,8.25336808851749));
#14267=CARTESIAN_POINT('Ctrl Pts',(-2.20385216862142,51.4130977477473,8.298050958181));
#14268=CARTESIAN_POINT('Ctrl Pts',(-2.51337907056068,50.7032211259283,8.34273382784451));
#14269=CARTESIAN_POINT('Ctrl Pts',(-2.51945660451951,49.9980217824357,8.38741669750802));
#14270=CARTESIAN_POINT('Origin',(0.,50.,5.));
#14271=CARTESIAN_POINT('',(-2.51977158007336,50.0018123497868,9.38741669750802));
#14272=CARTESIAN_POINT('',(-2.51421069693398,50.0014124180709,9.11258330249199));
#14273=CARTESIAN_POINT('',(-2.5175,50.,5.));
#14274=CARTESIAN_POINT('',(1.91346599666507,51.6359872033749,10.));
#14275=CARTESIAN_POINT('Ctrl Pts',(-2.51977158007336,50.0018123497868,9.38741669750802));
#14276=CARTESIAN_POINT('Ctrl Pts',(-2.51384336591692,49.2855430820957,9.43282641244633));
#14277=CARTESIAN_POINT('Ctrl Pts',(-2.19294820505509,48.5647754397593,9.47823612738464));
#14278=CARTESIAN_POINT('Ctrl Pts',(-1.65296056616486,48.0958821170945,9.52364584232295));
#14279=CARTESIAN_POINT('Ctrl Pts',(-1.02356671844595,47.5493537315036,9.57657408206485));
#14280=CARTESIAN_POINT('Ctrl Pts',(-0.0965236035471523,47.3450105607878,
9.62950232180674));
#14281=CARTESIAN_POINT('Ctrl Pts',(0.703763603554138,47.5780839006293,9.68243056154863));
#14282=CARTESIAN_POINT('Ctrl Pts',(1.50405081065543,47.8111572404708,9.73535880129053));
#14283=CARTESIAN_POINT('Ctrl Pts',(2.17758210995922,48.4816470908697,9.78828704103243));
#14284=CARTESIAN_POINT('Ctrl Pts',(2.41595103931381,49.2787700048902,9.84121528077432));
#14285=CARTESIAN_POINT('Ctrl Pts',(2.6543199686684,50.0758929189107,9.89414352051622));
#14286=CARTESIAN_POINT('Ctrl Pts',(2.45752652807378,50.9996488965529,9.94707176025811));
#14287=CARTESIAN_POINT('Ctrl Pts',(1.91346599666507,51.6359872033749,10.));
#14288=CARTESIAN_POINT('',(-1.91709562399829,51.6387694827081,10.));
#14289=CARTESIAN_POINT('Origin',(0.,50.,10.));
#14290=CARTESIAN_POINT('Ctrl Pts',(-1.91709820558801,51.6387714616175,10.));
#14291=CARTESIAN_POINT('Ctrl Pts',(-1.38628658638899,52.2578908816981,9.94821753066413));
#14292=CARTESIAN_POINT('Ctrl Pts',(-0.526694367197532,52.597340211881,9.89643506132826));
#14293=CARTESIAN_POINT('Ctrl Pts',(0.283636601049879,52.5054918828108,9.84465259199238));
#14294=CARTESIAN_POINT('Ctrl Pts',(1.11189744507203,52.4116112617576,9.79172435225049));
#14295=CARTESIAN_POINT('Ctrl Pts',(1.88869295170318,51.8671355152453,9.73879611250859));
#14296=CARTESIAN_POINT('Ctrl Pts',(2.2589558309103,51.1206234649951,9.6858678727667));
#14297=CARTESIAN_POINT('Ctrl Pts',(2.62921871011742,50.374111414745,9.6329396330248));
#14298=CARTESIAN_POINT('Ctrl Pts',(2.59294896190052,49.425563060757,9.58001139328291));
#14299=CARTESIAN_POINT('Ctrl Pts',(2.16649410945695,48.7095058870182,9.52708315354102));
#14300=CARTESIAN_POINT('Ctrl Pts',(1.74003925701338,47.9934487132793,9.47415491379912));
#14301=CARTESIAN_POINT('Ctrl Pts',(0.923399300343145,47.5098827197895,9.42122667405723));
#14302=CARTESIAN_POINT('Ctrl Pts',(0.0905131805637632,47.4799858088808,
9.36829843431533));
#14303=CARTESIAN_POINT('Ctrl Pts',(-0.742372939215617,47.4500888979721,
9.31537019457344));
#14304=CARTESIAN_POINT('Ctrl Pts',(-1.59150522210415,47.8738610696445,9.26244195483154));
#14305=CARTESIAN_POINT('Ctrl Pts',(-2.06826548542263,48.5574102936455,9.20951371508965));
#14306=CARTESIAN_POINT('Ctrl Pts',(-2.35930463112246,48.9746841260163,9.1772035775571));
#14307=CARTESIAN_POINT('Ctrl Pts',(-2.51157883686813,49.4887642305379,9.14489344002454));
#14308=CARTESIAN_POINT('Ctrl Pts',(-2.51421069693398,50.0014124180709,9.11258330249199));
#14309=CARTESIAN_POINT('Origin',(0.,50.,12.2084234471775));
#14310=CARTESIAN_POINT('',(-3.07857599143262,50.0001497381948,0.791576552822544));
#14311=CARTESIAN_POINT('',(-3.06854227339611,50.0007460267024,0.708423447177453));
#14312=CARTESIAN_POINT('',(-3.0735,50.0000000000001,12.2084234471775));
#14313=CARTESIAN_POINT('',(0.793799282532843,47.0307770462543,0.));
#14314=CARTESIAN_POINT('Ctrl Pts',(-3.06854227339611,50.0007460267024,0.708423447177453));
#14315=CARTESIAN_POINT('Ctrl Pts',(-3.06939439432918,50.4743080180887,0.683995257085881));
#14316=CARTESIAN_POINT('Ctrl Pts',(-2.74351660027806,51.9727061273031,0.606638827252413));
#14317=CARTESIAN_POINT('Ctrl Pts',(-0.409110687221481,53.6089533032289,
0.47635415767705));
#14318=CARTESIAN_POINT('Ctrl Pts',(2.81294218225317,52.3024584702958,0.317569438451368));
#14319=CARTESIAN_POINT('Ctrl Pts',(3.45486176146768,48.8813761711215,0.158784719225683));
#14320=CARTESIAN_POINT('Ctrl Pts',(1.78123794632758,47.2947612990625,0.0529282397418946));
#14321=CARTESIAN_POINT('Ctrl Pts',(0.793799282532844,47.0307770462543,0.));
#14322=CARTESIAN_POINT('',(-0.793799282532893,47.0307770462543,0.));
#14323=CARTESIAN_POINT('Origin',(0.,50.,0.));
#14324=CARTESIAN_POINT('Ctrl Pts',(-3.07857599143262,50.0001497381948,0.791576552822544));
#14325=CARTESIAN_POINT('Ctrl Pts',(-3.07858032390664,50.0071359194187,0.791213130185147));
#14326=CARTESIAN_POINT('Ctrl Pts',(-3.07539543013204,51.0315729209784,0.737921467805856));
#14327=CARTESIAN_POINT('Ctrl Pts',(-1.94901659367837,53.0656756689436,0.631701565684669));
#14328=CARTESIAN_POINT('Ctrl Pts',(1.51908697082356,53.300340014212,0.472916846458987));
#14329=CARTESIAN_POINT('Ctrl Pts',(3.59644503276003,50.5125594541255,0.314132127233302));
#14330=CARTESIAN_POINT('Ctrl Pts',(2.3901758303772,47.2810813042181,0.15649317841364));
#14331=CARTESIAN_POINT('Ctrl Pts',(0.166672989744518,46.7696415803318,0.051782469335873));
#14332=CARTESIAN_POINT('Ctrl Pts',(-0.795528245027205,47.0254639548254,
-4.66206934168767E-17));
#14333=CARTESIAN_POINT('Origin',(0.,50.,12.2084234471775));
#14334=CARTESIAN_POINT('',(-3.0714204791275,50.0025993512516,1.79157655282254));
#14335=CARTESIAN_POINT('',(-3.07330104137895,49.9971878127024,1.70842344717745));
#14336=CARTESIAN_POINT('',(-3.0735,50.0000000000001,12.2084234471775));
#14337=CARTESIAN_POINT('Ctrl Pts',(-3.07330104137895,49.9971878127024,1.70842344717745));
#14338=CARTESIAN_POINT('Ctrl Pts',(-3.06621203713203,50.7732867930175,1.66823136220391));
#14339=CARTESIAN_POINT('Ctrl Pts',(-2.37409258821072,52.5826738386258,1.57511103748848));
#14340=CARTESIAN_POINT('Ctrl Pts',(0.666391278186825,53.5712340631145,1.42906247303115));
#14341=CARTESIAN_POINT('Ctrl Pts',(3.36199101081887,51.3766498223304,1.27027775380547));
#14342=CARTESIAN_POINT('Ctrl Pts',(2.97966262373907,47.9216585932218,1.11149303457979));
#14343=CARTESIAN_POINT('Ctrl Pts',(-0.130337674918302,46.3695658811752,
0.952708315354101));
#14344=CARTESIAN_POINT('Ctrl Pts',(-2.66118372910024,47.8681845578855,0.818351786219992));
#14345=CARTESIAN_POINT('Ctrl Pts',(-3.06754811505652,49.4482474495905,0.736923496827775));
#14346=CARTESIAN_POINT('Ctrl Pts',(-3.06854227339611,50.0007460267024,0.708423447177453));
#14347=CARTESIAN_POINT('Ctrl Pts',(-3.0714204791275,50.0025993512516,1.79157655282254));
#14348=CARTESIAN_POINT('Ctrl Pts',(-3.07392356725168,50.3144977337562,1.77544923530318));
#14349=CARTESIAN_POINT('Ctrl Pts',(-2.88682155748466,51.6470826375239,1.70639367804192));
#14350=CARTESIAN_POINT('Ctrl Pts',(-0.965959409052926,53.5021157627911,
1.58440988103877));
#14351=CARTESIAN_POINT('Ctrl Pts',(2.41872209844688,52.7106678650022,1.42562516181309));
#14352=CARTESIAN_POINT('Ctrl Pts',(3.58910270149602,49.4376309512673,1.2668404425874));
#14353=CARTESIAN_POINT('Ctrl Pts',(1.47372061005109,46.6794679460814,1.10805572336172));
#14354=CARTESIAN_POINT('Ctrl Pts',(-1.98290181661967,46.9604846321805,0.949634426773433));
#14355=CARTESIAN_POINT('Ctrl Pts',(-3.0779493499385,48.9896806575687,0.844141369927042));
#14356=CARTESIAN_POINT('Ctrl Pts',(-3.07857599143262,50.0001497381948,0.791576552822544));
#14357=CARTESIAN_POINT('Origin',(0.,50.,12.2084234471775));
#14358=CARTESIAN_POINT('',(-3.06935579216157,49.998376067411,2.79157655282254));
#14359=CARTESIAN_POINT('',(-3.07814148031383,50.0010564595264,2.70842344717745));
#14360=CARTESIAN_POINT('',(-3.0735,50.0000000000001,12.2084234471775));
#14361=CARTESIAN_POINT('Ctrl Pts',(-3.07814148031383,50.0010564595264,2.70842344717745));
#14362=CARTESIAN_POINT('Ctrl Pts',(-3.07840095523816,50.0592826774211,2.70539570706384));
#14363=CARTESIAN_POINT('Ctrl Pts',(-3.05051243711967,51.1351139926954,2.64943972720834));
#14364=CARTESIAN_POINT('Ctrl Pts',(-1.79264823311626,53.1597984449186,2.54055550761094));
#14365=CARTESIAN_POINT('Ctrl Pts',(1.68282148580427,53.2196308819302,2.38177078838525));
#14366=CARTESIAN_POINT('Ctrl Pts',(3.61769661596932,50.3319453337173,2.22298606915957));
#14367=CARTESIAN_POINT('Ctrl Pts',(2.24062890528198,47.1403675327308,2.06420134993389));
#14368=CARTESIAN_POINT('Ctrl Pts',(-1.1876948837818,46.5667395440464,1.9054166307082));
#14369=CARTESIAN_POINT('Ctrl Pts',(-2.93614411454864,48.4858084944497,1.78682399645606));
#14370=CARTESIAN_POINT('Ctrl Pts',(-3.07554742036879,49.7512558901519,1.72115960194581));
#14371=CARTESIAN_POINT('Ctrl Pts',(-3.07330104137895,49.9971878127024,1.70842344717745));
#14372=CARTESIAN_POINT('Ctrl Pts',(-3.06935579216157,49.998376067411,2.79157655282254));
#14373=CARTESIAN_POINT('Ctrl Pts',(-3.06639561916484,50.6161884641465,2.75968534042121));
#14374=CARTESIAN_POINT('Ctrl Pts',(-2.58560749438489,52.2635918629999,2.67486588827799));
#14375=CARTESIAN_POINT('Ctrl Pts',(0.101753748544503,53.6314673752793,2.53711819639287));
#14376=CARTESIAN_POINT('Ctrl Pts',(3.10637882983628,51.8836985739372,2.37833347716719));
#14377=CARTESIAN_POINT('Ctrl Pts',(3.26716539423699,48.4114345548525,2.2195487579415));
#14378=CARTESIAN_POINT('Ctrl Pts',(0.436916036883408,46.3934765333616,2.06076403871582));
#14379=CARTESIAN_POINT('Ctrl Pts',(-2.46523651005939,47.546842799228,1.9181066370095));
#14380=CARTESIAN_POINT('Ctrl Pts',(-3.06570868289955,49.2908785023193,1.82837747504507));
#14381=CARTESIAN_POINT('Ctrl Pts',(-3.0714204791275,50.0025993512516,1.79157655282254));
#14382=CARTESIAN_POINT('Origin',(0.,50.,12.2084234471775));
#14383=CARTESIAN_POINT('',(-3.07734549507316,49.9982621438963,3.79157655282254));
#14384=CARTESIAN_POINT('',(-3.07017362606608,50.0021532365281,3.70842344717745));
#14385=CARTESIAN_POINT('',(-3.0735,50.0000000000001,12.2084234471775));
#14386=CARTESIAN_POINT('Ctrl Pts',(-3.07017362606608,50.0021532365281,3.70842344717745));
#14387=CARTESIAN_POINT('Ctrl Pts',(-3.07252461422455,50.3659511320327,3.68963181218188));
#14388=CARTESIAN_POINT('Ctrl Pts',(-2.84443426502969,51.7515648716753,3.61791193744441));
#14389=CARTESIAN_POINT('Ctrl Pts',(-0.788934856752224,53.54619447354,3.49326382296504));
#14390=CARTESIAN_POINT('Ctrl Pts',(2.551748227883,52.5858256675908,3.33447910373936));
#14391=CARTESIAN_POINT('Ctrl Pts',(3.5563479740914,49.2581761937472,3.17569438451367));
#14392=CARTESIAN_POINT('Ctrl Pts',(1.30516987545015,46.6096541304332,3.01690966528799));
#14393=CARTESIAN_POINT('Ctrl Pts',(-2.07515983968236,47.0562563206458,2.86115268617591));
#14394=CARTESIAN_POINT('Ctrl Pts',(-3.07386504710643,49.0414241082048,2.75832394680574));
#14395=CARTESIAN_POINT('Ctrl Pts',(-3.07814148031383,50.0010564595264,2.70842344717745));
#14396=CARTESIAN_POINT('Ctrl Pts',(-3.07734549507316,49.9982621438963,3.79157655282254));
#14397=CARTESIAN_POINT('Ctrl Pts',(-3.0711410240522,50.9153404750885,3.74392144553925));
#14398=CARTESIAN_POINT('Ctrl Pts',(-2.14944206797417,52.8617971516187,3.64333809851406));
#14399=CARTESIAN_POINT('Ctrl Pts',(1.160548502562,53.4425334553022,3.48982651174698));
#14400=CARTESIAN_POINT('Ctrl Pts',(3.52177447035456,50.8916355787576,3.33104179252129));
#14401=CARTESIAN_POINT('Ctrl Pts',(2.65887408716728,47.524460054095,3.17225707329561));
#14402=CARTESIAN_POINT('Ctrl Pts',(-0.638181599955106,46.4236004656121,
3.01347235406992));
#14403=CARTESIAN_POINT('Ctrl Pts',(-2.80613642398289,48.1603828111261,2.88657884724557));
#14404=CARTESIAN_POINT('Ctrl Pts',(-3.07130846926525,49.5908363314516,2.81261358016311));
#14405=CARTESIAN_POINT('Ctrl Pts',(-3.06935579216157,49.998376067411,2.79157655282254));
#14406=CARTESIAN_POINT('Origin',(0.,50.,12.2084234471775));
#14407=CARTESIAN_POINT('',(-3.07461570809594,50.002710506979,4.79157655282254));
#14408=CARTESIAN_POINT('',(-3.07035160721926,49.9977623829844,4.70842344717745));
#14409=CARTESIAN_POINT('',(-3.0735,50.0000000000001,12.2084234471775));
#14410=CARTESIAN_POINT('Ctrl Pts',(-3.07035160721926,49.9977623829844,4.70842344717746));
#14411=CARTESIAN_POINT('Ctrl Pts',(-3.06584225025972,50.6666449550227,4.67386791729991));
#14412=CARTESIAN_POINT('Ctrl Pts',(-2.52195697727917,52.3667212082676,4.58638414768047));
#14413=CARTESIAN_POINT('Ctrl Pts',(0.283925502051857,53.621781295074,4.44597213831914));
#14414=CARTESIAN_POINT('Ctrl Pts',(3.19702456896977,51.7253832457192,4.28718741909346));
#14415=CARTESIAN_POINT('Ctrl Pts',(3.18330045542969,48.2494253370868,4.12840269986777));
#14416=CARTESIAN_POINT('Ctrl Pts',(0.255317360099809,46.3760896137859,3.96961798064209));
#14417=CARTESIAN_POINT('Ctrl Pts',(-2.53222545405911,47.6494566272368,3.82962489641198));
#14418=CARTESIAN_POINT('Ctrl Pts',(-3.06590285593096,49.3412833883586,3.74256005192377));
#14419=CARTESIAN_POINT('Ctrl Pts',(-3.07017362606608,50.0021532365281,3.70842344717745));
#14420=CARTESIAN_POINT('Ctrl Pts',(-3.07461570809594,50.002710506979,4.79157655282255));
#14421=CARTESIAN_POINT('Ctrl Pts',(-3.07647553176869,50.205062018161,4.78108579039918));
#14422=CARTESIAN_POINT('Ctrl Pts',(-2.96604334544996,51.4263020184257,4.71766678823391));
#14423=CARTESIAN_POINT('Ctrl Pts',(-1.33190075959052,53.3799334001034,4.60131954632676));
#14424=CARTESIAN_POINT('Ctrl Pts',(2.1176259614783,52.951875625715,4.44253482710107));
#14425=CARTESIAN_POINT('Ctrl Pts',(3.62850109627196,49.8214244786094,4.28375010787539));
#14426=CARTESIAN_POINT('Ctrl Pts',(1.81754341731002,46.8544562713326,4.12496538864971));
#14427=CARTESIAN_POINT('Ctrl Pts',(-1.65734523585442,46.76718138599,3.96618066942402));
#14428=CARTESIAN_POINT('Ctrl Pts',(-3.02743399158457,48.7774471850316,3.85505105748164));
#14429=CARTESIAN_POINT('Ctrl Pts',(-3.07803203213905,49.8967856014863,3.79684968528114));
#14430=CARTESIAN_POINT('Ctrl Pts',(-3.07734549507316,49.9982621438963,3.79157655282254));
#14431=CARTESIAN_POINT('Origin',(0.,50.,12.2084234471775));
#14432=CARTESIAN_POINT('',(-3.06849806069028,50.0000666768364,5.79157655282255));
#14433=CARTESIAN_POINT('',(-3.0782507036788,49.9990828923494,5.70842344717746));
#14434=CARTESIAN_POINT('',(-3.0735,50.0000000000001,12.2084234471775));
#14435=CARTESIAN_POINT('Ctrl Pts',(-3.0782507036788,49.9990828923494,5.70842344717746));
#14436=CARTESIAN_POINT('Ctrl Pts',(-3.07444452114988,50.9666800272788,5.65810402241794));
#14437=CARTESIAN_POINT('Ctrl Pts',(-2.06095094116992,52.9589090168758,5.55485635791654));
#14438=CARTESIAN_POINT('Ctrl Pts',(1.3319009622986,53.3799339145109,5.39868045367324));
#14439=CARTESIAN_POINT('Ctrl Pts',(3.56209487930137,50.7137180890468,5.23989573444756));
#14440=CARTESIAN_POINT('Ctrl Pts',(2.53124977721441,47.3941051431169,5.08111101522187));
#14441=CARTESIAN_POINT('Ctrl Pts',(-0.816912681732443,46.460145891388,4.92232629599619));
#14442=CARTESIAN_POINT('Ctrl Pts',(-2.85131635541723,48.2648648637016,4.79809710664805));
#14443=CARTESIAN_POINT('Ctrl Pts',(-3.07274917158553,49.6421265275098,4.72679615704181));
#14444=CARTESIAN_POINT('Ctrl Pts',(-3.07035160721926,49.9977623829844,4.70842344717746));
#14445=CARTESIAN_POINT('Ctrl Pts',(-3.06849806069028,50.0000666768364,5.79157655282255));
#14446=CARTESIAN_POINT('Ctrl Pts',(-3.0685965252858,50.5090402624651,5.76532189551721));
#14447=CARTESIAN_POINT('Ctrl Pts',(-2.70766479984231,52.0439509300286,5.68613899846998));
#14448=CARTESIAN_POINT('Ctrl Pts',(-0.283925458840122,53.6217807438589,
5.55402786168086));
#14449=CARTESIAN_POINT('Ctrl Pts',(2.889102232167,52.2024980623317,5.39524314245518));
#14450=CARTESIAN_POINT('Ctrl Pts',(3.41720455519345,48.7668647882805,5.23645842322949));
#14451=CARTESIAN_POINT('Ctrl Pts',(0.816912557402795,46.4601464301344,5.07767370400381));
#14452=CARTESIAN_POINT('Ctrl Pts',(-2.3100393678769,47.3323997082042,4.92937974720149));
#14453=CARTESIAN_POINT('Ctrl Pts',(-3.06709230591183,49.1841534450989,4.83401403014107));
#14454=CARTESIAN_POINT('Ctrl Pts',(-3.07461570809594,50.002710506979,4.79157655282255));
#14455=CARTESIAN_POINT('Origin',(0.,50.,12.2084234471775));
#14456=CARTESIAN_POINT('',(-3.07437087614155,49.9972554431979,6.79157655282255));
#14457=CARTESIAN_POINT('',(-3.0730581170342,50.0028093778768,6.70842344717746));
#14458=CARTESIAN_POINT('',(-3.0735,50.0000000000001,12.2084234471775));
#14459=CARTESIAN_POINT('Ctrl Pts',(-3.0730581170342,50.0028093778768,6.70842344717746));
#14460=CARTESIAN_POINT('Ctrl Pts',(-3.07535959640269,50.2568814410373,6.69526836727788));
#14461=CARTESIAN_POINT('Ctrl Pts',(-2.93032368413276,51.5305969754684,6.6291850476364));
#14462=CARTESIAN_POINT('Ctrl Pts',(-1.16054867919063,53.4425339792431,6.51017348825302));
#14463=CARTESIAN_POINT('Ctrl Pts',(2.26314079233676,52.8418492563365,6.35138876902735));
#14464=CARTESIAN_POINT('Ctrl Pts',(3.6149622537802,49.6394984830586,6.19260404980166));
#14465=CARTESIAN_POINT('Ctrl Pts',(1.65734548809325,46.7671808939717,6.03381933057597));
#14466=CARTESIAN_POINT('Ctrl Pts',(-1.81754369393026,46.8544557925985,5.87503461135029));
#14467=CARTESIAN_POINT('Ctrl Pts',(-3.05460283140418,48.8811818580631,5.76656931688412));
#14468=CARTESIAN_POINT('Ctrl Pts',(-3.07844803554526,49.9489177341708,5.71103226215984));
#14469=CARTESIAN_POINT('Ctrl Pts',(-3.0782507036788,49.9990828923494,5.70842344717746));
#14470=CARTESIAN_POINT('Ctrl Pts',(-3.07437087614155,49.9972554431979,6.79157655282255));
#14471=CARTESIAN_POINT('Ctrl Pts',(-3.06689206860327,50.8078980828033,6.74955800063525));
#14472=CARTESIAN_POINT('Ctrl Pts',(-2.32221817630179,52.6518097217997,6.65461120870605));
#14473=CARTESIAN_POINT('Ctrl Pts',(0.788934736670248,53.5461939338473,6.50673617703496));
#14474=CARTESIAN_POINT('Ctrl Pts',(3.40736059977763,51.2600806198138,6.34795145780928));
#14475=CARTESIAN_POINT('Ctrl Pts',(2.90640411768017,47.8203843177281,6.1891667385836));
#14476=CARTESIAN_POINT('Ctrl Pts',(-0.255317321240407,46.3760901653225,
6.03038201935791));
#14477=CARTESIAN_POINT('Ctrl Pts',(-2.69916534238486,47.939674261022,5.89785195743756));
#14478=CARTESIAN_POINT('Ctrl Pts',(-3.06839802497186,49.482971795863,5.81825013525911));
#14479=CARTESIAN_POINT('Ctrl Pts',(-3.06849806069028,50.0000666768364,5.79157655282255));
#14480=CARTESIAN_POINT('Origin',(0.,50.,12.2084234471775));
#14481=CARTESIAN_POINT('',(-3.07751802765106,50.0016205064162,7.79157655282255));
#14482=CARTESIAN_POINT('',(-3.06867630081942,49.9992281639212,7.70842344717746));
#14483=CARTESIAN_POINT('',(-3.0735,50.0000000000001,12.2084234471775));
#14484=CARTESIAN_POINT('Ctrl Pts',(-3.06867630081942,49.9992281639212,7.70842344717746));
#14485=CARTESIAN_POINT('Ctrl Pts',(-3.0674168112757,50.559771360493,7.67950447239591));
#14486=CARTESIAN_POINT('Ctrl Pts',(-2.65206070693095,52.1479727200386,7.59765725787247));
#14487=CARTESIAN_POINT('Ctrl Pts',(-0.101753763996771,53.6314679282393,
7.46288180360713));
#14488=CARTESIAN_POINT('Ctrl Pts',(2.99602565802517,52.0546882429035,7.30409708438145));
#14489=CARTESIAN_POINT('Ctrl Pts',(3.3509930854224,48.5968753391809,7.14531236515576));
#14490=CARTESIAN_POINT('Ctrl Pts',(0.638181697078704,46.4235999212631,6.98652764593008));
#14491=CARTESIAN_POINT('Ctrl Pts',(-2.38571824726309,47.4332550695025,6.84089800660398));
#14492=CARTESIAN_POINT('Ctrl Pts',(-3.06609980834313,49.2346461392885,6.74819660701977));
#14493=CARTESIAN_POINT('Ctrl Pts',(-3.0730581170342,50.0028093778768,6.70842344717746));
#14494=CARTESIAN_POINT('Ctrl Pts',(-3.07751802765106,50.0016205064162,7.79157655282255));
#14495=CARTESIAN_POINT('Ctrl Pts',(-3.07811546112488,50.095021443553,7.78672234549518));
#14496=CARTESIAN_POINT('Ctrl Pts',(-3.03188884220289,51.2062275721529,7.72893989842591));
#14497=CARTESIAN_POINT('Ctrl Pts',(-1.68282122891848,53.2196303903089,7.61822921161475));
#14498=CARTESIAN_POINT('Ctrl Pts',(1.79264795986253,53.1597979648733,7.45944449238905));
#14499=CARTESIAN_POINT('Ctrl Pts',(3.62697790104741,50.2072222411372,7.30065977316339));
#14500=CARTESIAN_POINT('Ctrl Pts',(2.14086931327707,47.0649382107817,7.14187505393769));
#14501=CARTESIAN_POINT('Ctrl Pts',(-1.30516967674285,46.6096546462972,6.98309033471202));
#14502=CARTESIAN_POINT('Ctrl Pts',(-2.96062745118739,48.5573088293533,6.86632416767363));
#14503=CARTESIAN_POINT('Ctrl Pts',(-3.07631267206921,49.7867803683524,6.80248624037714));
#14504=CARTESIAN_POINT('Ctrl Pts',(-3.07437087614155,49.9972554431979,6.79157655282255));
#14505=CARTESIAN_POINT('Origin',(0.,50.,12.2084234471775));
#14506=CARTESIAN_POINT('',(-3.06948424112278,50.0017243562825,8.79157655282255));
#14507=CARTESIAN_POINT('',(-3.0758887284968,49.9975848851305,8.70842344717746));
#14508=CARTESIAN_POINT('',(-3.0735,50.0000000000001,12.2084234471775));
#14509=CARTESIAN_POINT('Ctrl Pts',(-3.0758887284968,49.9975848851305,8.70842344717746));
#14510=CARTESIAN_POINT('Ctrl Pts',(-3.06846894672027,50.8585303398374,8.66374057751394));
#14511=CARTESIAN_POINT('Ctrl Pts',(-2.24296276284576,52.7517665575233,8.56612946810853));
#14512=CARTESIAN_POINT('Ctrl Pts',(0.965959558335722,53.5021163068972,8.41559011896124));
#14513=CARTESIAN_POINT('Ctrl Pts',(3.4663211670797,51.087443472416,8.25680539973554));
#14514=CARTESIAN_POINT('Ctrl Pts',(2.79332321135939,47.6772296827595,8.09802068050987));
#14515=CARTESIAN_POINT('Ctrl Pts',(-0.436916103658114,46.3934759827048,
7.93923596128417));
#14516=CARTESIAN_POINT('Ctrl Pts',(-2.75170116252904,48.0439097412714,7.80937021684004));
#14517=CARTESIAN_POINT('Ctrl Pts',(-3.06972196092315,49.533851011727,7.7324327121378));
#14518=CARTESIAN_POINT('Ctrl Pts',(-3.06867630081942,49.9992281639212,7.70842344717746));
#14519=CARTESIAN_POINT('Ctrl Pts',(-3.06948424112278,50.0017243562825,8.79157655282255));
#14520=CARTESIAN_POINT('Ctrl Pts',(-3.07153463083539,50.4011105484092,8.77095845061321));
#14521=CARTESIAN_POINT('Ctrl Pts',(-2.81347939940506,51.823212235849,8.69741210866198));
#14522=CARTESIAN_POINT('Ctrl Pts',(-0.666391154437672,53.5712334545473,
8.57093752696884));
#14523=CARTESIAN_POINT('Ctrl Pts',(2.63923735448624,52.496466169517,8.41215280774317));
#14524=CARTESIAN_POINT('Ctrl Pts',(3.52870838065631,49.1361979230418,8.25336808851748));
#14525=CARTESIAN_POINT('Ctrl Pts',(1.18769469860156,46.5667400770053,8.0945833692918));
#14526=CARTESIAN_POINT('Ctrl Pts',(-2.13582129838156,47.1228315854216,7.94065285739348));
#14527=CARTESIAN_POINT('Ctrl Pts',(-3.0716012972255,49.0766168185547,7.83965058523707));
#14528=CARTESIAN_POINT('Ctrl Pts',(-3.07751802765106,50.0016205064162,7.79157655282255));
#14529=CARTESIAN_POINT('Origin',(0.,50.,12.2084234471775));
#14530=CARTESIAN_POINT('',(-3.0704093202101,49.9964518649217,9.79157655282255));
#14531=CARTESIAN_POINT('',(-3.07627326766851,50.0022126145262,9.70842344717746));
#14532=CARTESIAN_POINT('',(-3.0735,50.0000000000001,12.2084234471775));
#14533=CARTESIAN_POINT('',(-0.79379928253289,47.0307770462543,10.));
#14534=CARTESIAN_POINT('Ctrl Pts',(-0.79379928253289,47.0307770462543,10.));
#14535=CARTESIAN_POINT('Ctrl Pts',(-1.78123794632762,47.2947612990625,9.94707176025811));
#14536=CARTESIAN_POINT('Ctrl Pts',(-2.87965183287623,48.3360650844884,9.87759727786562));
#14537=CARTESIAN_POINT('Ctrl Pts',(-3.07283314005625,49.6763547812676,9.80812279547314));
#14538=CARTESIAN_POINT('Ctrl Pts',(-3.0704093202101,49.9964518649217,9.79157655282255));
#14539=CARTESIAN_POINT('',(0.795527717319754,47.0254679690975,10.));
#14540=CARTESIAN_POINT('Origin',(0.,50.,10.));
#14541=CARTESIAN_POINT('Ctrl Pts',(0.79552895279625,47.0254641741959,10.));
#14542=CARTESIAN_POINT('Ctrl Pts',(-0.166671812615051,46.7696422359245,
9.94821753066412));
#14543=CARTESIAN_POINT('Ctrl Pts',(-2.23052341514648,47.2443566461646,9.85102534638995));
#14544=CARTESIAN_POINT('Ctrl Pts',(-3.06903578357325,49.12775239834,9.75383316211577));
#14545=CARTESIAN_POINT('Ctrl Pts',(-3.07627326766851,50.0022126145262,9.70842344717746));
#14546=CARTESIAN_POINT('Origin',(-5.55111512312578E-16,7.54951656745106E-14,
4.));
#14547=CARTESIAN_POINT('',(-7.44220860705898,25.9540657903346,4.));
#14548=CARTESIAN_POINT('',(7.44220860705898,25.9540657903346,4.));
#14549=CARTESIAN_POINT('Origin',(-5.55111512312578E-16,7.54951656745106E-14,
4.));
#14550=CARTESIAN_POINT('',(-7.44220860705898,25.9540657903346,0.));
#14551=CARTESIAN_POINT('',(-7.44220860705898,25.9540657903346,4.));
#14552=CARTESIAN_POINT('',(7.44220860705898,25.9540657903346,0.));
#14553=CARTESIAN_POINT('Origin',(-5.55111512312578E-16,7.54951656745106E-14,
0.));
#14554=CARTESIAN_POINT('',(7.44220860705898,25.9540657903346,4.));
#14555=CARTESIAN_POINT('Origin',(-6.89093389542498,24.031542398458,4.));
#14556=CARTESIAN_POINT('',(-6.33965915514315,22.109019014796,4.));
#14557=CARTESIAN_POINT('Origin',(-6.89093389542498,24.031542398458,4.));
#14558=CARTESIAN_POINT('',(-6.33965915514315,22.109019014796,0.));
#14559=CARTESIAN_POINT('',(-6.33965915514315,22.109019014796,4.));
#14560=CARTESIAN_POINT('Origin',(-6.89093389542498,24.031542398458,0.));
#14561=CARTESIAN_POINT('Origin',(0.,-1.06581410364015E-13,4.));
#14562=CARTESIAN_POINT('',(6.33965918379098,22.1090190065813,4.));
#14563=CARTESIAN_POINT('Origin',(0.,-1.06581410364015E-13,4.));
#14564=CARTESIAN_POINT('',(6.33965918379098,22.1090190065813,0.));
#14565=CARTESIAN_POINT('',(6.33965918379098,22.1090190065813,4.));
#14566=CARTESIAN_POINT('Origin',(0.,-1.06581410364015E-13,0.));
#14567=CARTESIAN_POINT('Origin',(6.89093389542498,24.031542398458,4.));
#14568=CARTESIAN_POINT('Origin',(6.89093389542498,24.031542398458,4.));
#14569=CARTESIAN_POINT('Origin',(6.89093389542498,24.031542398458,0.));
#14570=CARTESIAN_POINT('Origin',(0.,50.,12.2084234471775));
#14571=CARTESIAN_POINT('Ctrl Pts',(-3.07627326766851,50.0022126145262,9.70842344717746));
#14572=CARTESIAN_POINT('Ctrl Pts',(-3.07747158401468,50.1469977300918,9.70090492237387));
#14573=CARTESIAN_POINT('Ctrl Pts',(-3.00235625554453,51.3098177813352,9.64045815782839));
#14574=CARTESIAN_POINT('Ctrl Pts',(-1.5190875024664,53.3003399032799,9.52708315354102));
#14575=CARTESIAN_POINT('Ctrl Pts',(1.94901703988696,53.0656764961195,9.36829843431533));
#14576=CARTESIAN_POINT('Ctrl Pts',(3.63280460830591,50.0249606151346,9.20951371508965));
#14577=CARTESIAN_POINT('Ctrl Pts',(1.99083173979432,46.9611289474581,9.05072899586396));
#14578=CARTESIAN_POINT('Ctrl Pts',(-1.4737208527869,46.6794673744635,8.89194427663828));
#14579=CARTESIAN_POINT('Ctrl Pts',(-2.99382331557603,48.6614689264833,8.77784242707612));
#14580=CARTESIAN_POINT('Ctrl Pts',(-3.07725790749334,49.8387138469717,8.71666881725584));
#14581=CARTESIAN_POINT('Ctrl Pts',(-3.0758887284968,49.9975848851305,8.70842344717746));
#14582=CARTESIAN_POINT('Ctrl Pts',(-3.0704093202101,49.9964518649217,9.79157655282255));
#14583=CARTESIAN_POINT('Ctrl Pts',(-3.06507980773682,50.7002836297739,9.75519455573125));
#14584=CARTESIAN_POINT('Ctrl Pts',(-2.47718564593827,52.4386050547508,9.66588431889805));
#14585=CARTESIAN_POINT('Ctrl Pts',(0.409110549274297,53.6089507129763,9.52364584232294));
#14586=CARTESIAN_POINT('Ctrl Pts',(3.25417230454442,51.6147744981929,9.36486112309727));
#14587=CARTESIAN_POINT('Ctrl Pts',(3.12133210059845,48.1406572795451,9.20607640387158));
#14588=CARTESIAN_POINT('Ctrl Pts',(0.130337574092825,46.3695668156037,9.0472916846459));
#14589=CARTESIAN_POINT('Ctrl Pts',(-2.57583048728707,47.7201204800813,8.90912506762955));
#14590=CARTESIAN_POINT('Ctrl Pts',(-3.06627112417646,49.3758557547402,8.82388669035511));
#14591=CARTESIAN_POINT('Ctrl Pts',(-3.06948424112278,50.0017243562825,8.79157655282255));
#14592=CARTESIAN_POINT('Ctrl Pts',(1.91346599666507,51.6359872033749,10.));
#14593=CARTESIAN_POINT('Ctrl Pts',(2.45752652807378,50.9996488965529,9.94707176025811));
#14594=CARTESIAN_POINT('Ctrl Pts',(2.85111340926301,49.1521369412685,9.84121528077433));
#14595=CARTESIAN_POINT('Ctrl Pts',(0.83051951135165,47.140667390072,9.68243056154863));
#14596=CARTESIAN_POINT('Ctrl Pts',(-1.95060983334475,47.7536969022194,9.52364584232296));
#14597=CARTESIAN_POINT('Ctrl Pts',(-2.94584357496186,50.4198377036174,9.36486112309726));
#14598=CARTESIAN_POINT('Ctrl Pts',(-1.24428267039504,52.7033042806271,9.20607640387159));
#14599=CARTESIAN_POINT('Ctrl Pts',(1.59643741594775,52.5110917777716,9.0472916846459));
#14600=CARTESIAN_POINT('Ctrl Pts',(2.97562570405406,50.02044520859,8.88850696542022));
#14601=CARTESIAN_POINT('Ctrl Pts',(1.63068778426296,47.5108645274852,8.72972224619453));
#14602=CARTESIAN_POINT('Ctrl Pts',(-1.20712290447081,47.2801558858669,8.57093752696885));
#14603=CARTESIAN_POINT('Ctrl Pts',(-2.93982996683955,49.5393641766748,8.41215280774316));
#14604=CARTESIAN_POINT('Ctrl Pts',(-1.98117254630264,52.2203049740253,8.25336808851749));
#14605=CARTESIAN_POINT('Ctrl Pts',(0.791216264229766,52.8685790800761,8.09458336929179));
#14606=CARTESIAN_POINT('Ctrl Pts',(2.83925932589008,50.8907235860768,7.93579865006612));
#14607=CARTESIAN_POINT('Ctrl Pts',(2.28800754338613,48.0974217427516,7.77701393084044));
#14608=CARTESIAN_POINT('Ctrl Pts',(-0.357877433206215,47.0459006951226,
7.61822921161474));
#14609=CARTESIAN_POINT('Ctrl Pts',(-2.67613148900519,48.6988078365273,7.45944449238906));
#14610=CARTESIAN_POINT('Ctrl Pts',(-2.54443139563822,51.5429353767203,7.30065977316338));
#14611=CARTESIAN_POINT('Ctrl Pts',(-0.0833463806285565,52.9745308310859,
7.14187505393769));
#14612=CARTESIAN_POINT('Ctrl Pts',(2.45404086353615,51.6829925659703,6.98309033471202));
#14613=CARTESIAN_POINT('Ctrl Pts',(2.74479423866956,48.8507023479382,6.82430561548632));
#14614=CARTESIAN_POINT('Ctrl Pts',(0.522733828662967,47.0705751754612,6.66552089626065));
#14615=CARTESIAN_POINT('Ctrl Pts',(-2.1778807656371,47.9722880226893,6.50673617703496));
#14616=CARTESIAN_POINT('Ctrl Pts',(-2.88468149617291,50.730337696803,6.34795145780928));
#14617=CARTESIAN_POINT('Ctrl Pts',(-0.950603969371205,52.8197752701299,
6.18916673858359));
#14618=CARTESIAN_POINT('Ctrl Pts',(1.85373578809429,52.3277551660412,6.03038201935791));
#14619=CARTESIAN_POINT('Ctrl Pts',(2.96101105381215,49.7047136590531,5.87159730013223));
#14620=CARTESIAN_POINT('Ctrl Pts',(1.35752961323402,47.3520019198223,5.71281258090655));
#14621=CARTESIAN_POINT('Ctrl Pts',(-1.48874776296386,47.4234886799631,5.55402786168086));
#14622=CARTESIAN_POINT('Ctrl Pts',(-2.97210115507541,49.8537289918586,5.39524314245518));
#14623=CARTESIAN_POINT('Ctrl Pts',(-1.7345450364046,52.4178779953631,5.23645842322949));
#14624=CARTESIAN_POINT('Ctrl Pts',(1.09095840982161,52.7684996355234,5.07767370400381));
#14625=CARTESIAN_POINT('Ctrl Pts',(2.91770745360052,50.5846055927038,4.91888898477812));
#14626=CARTESIAN_POINT('Ctrl Pts',(2.07334352176257,47.8655147869845,4.76010426555244));
#14627=CARTESIAN_POINT('Ctrl Pts',(-0.669132154306629,47.1005099338114,
4.60131954632676));
#14628=CARTESIAN_POINT('Ctrl Pts',(-2.79902839661656,48.9899403390338,4.44253482710108));
#14629=CARTESIAN_POINT('Ctrl Pts',(-2.3664603795149,51.8040636784796,4.28375010787539));
#14630=CARTESIAN_POINT('Ctrl Pts',(0.232563023073223,52.966596521994,4.12496538864971));
#14631=CARTESIAN_POINT('Ctrl Pts',(2.61867881971088,51.4132592552783,3.96618066942402));
#14632=CARTESIAN_POINT('Ctrl Pts',(2.60743741550163,48.5661064864539,3.80739595019834));
#14633=CARTESIAN_POINT('Ctrl Pts',(0.209130129836104,47.03165954212,3.64861123097265));
#14634=CARTESIAN_POINT('Ctrl Pts',(-2.3806323344251,48.2146792532123,3.48982651174698));
#14635=CARTESIAN_POINT('Ctrl Pts',(-2.79096522383464,51.0321306143504,3.33104179252129));
#14636=CARTESIAN_POINT('Ctrl Pts',(-0.646215552911574,52.9046834511589,
3.17225707329561));
#14637=CARTESIAN_POINT('Ctrl Pts',(2.09013377702796,52.1180465652057,3.01347235406992));
#14638=CARTESIAN_POINT('Ctrl Pts',(2.91300017074186,49.3923730495392,2.85468763484424));
#14639=CARTESIAN_POINT('Ctrl Pts',(1.06906301006856,47.2229719451328,2.69590291561855));
#14640=CARTESIAN_POINT('Ctrl Pts',(-1.75358363974743,47.5958941989475,2.53711819639287));
#14641=CARTESIAN_POINT('Ctrl Pts',(-2.97085350739628,50.1697355043467,2.37833347716719));
#14642=CARTESIAN_POINT('Ctrl Pts',(-1.46835592219625,52.5881869481317,2.21954875794151));
#14643=CARTESIAN_POINT('Ctrl Pts',(1.37839697104677,52.6371956223391,2.06076403871582));
#14644=CARTESIAN_POINT('Ctrl Pts',(2.96325076645608,50.2718960070387,1.90197931949014));
#14645=CARTESIAN_POINT('Ctrl Pts',(1.83529632960708,47.65767862816,1.74319460026445));
#14646=CARTESIAN_POINT('Ctrl Pts',(-0.972839391547319,47.1878206611801,
1.58440988103877));
#14647=CARTESIAN_POINT('Ctrl Pts',(-2.89036104794741,49.2924607089264,1.42562516181309));
#14648=CARTESIAN_POINT('Ctrl Pts',(-2.16179635093426,52.0448525943808,1.2668404425874));
#14649=CARTESIAN_POINT('Ctrl Pts',(0.545840261212082,52.9251933476136,1.10805572336172));
#14650=CARTESIAN_POINT('Ctrl Pts',(2.75380262558533,51.1276121450193,0.949271004136036));
#14651=CARTESIAN_POINT('Ctrl Pts',(2.44063792264946,48.297633157129,0.790486284910355));
#14652=CARTESIAN_POINT('Ctrl Pts',(-0.106759426258933,47.0263159609106,
0.631701565684669));
#14653=CARTESIAN_POINT('Ctrl Pts',(-2.55667952108434,48.4770150283179,0.472916846458987));
#14654=CARTESIAN_POINT('Ctrl Pts',(-2.665488928155,51.3226590034494,0.314132127233303));
#14655=CARTESIAN_POINT('Ctrl Pts',(-0.335102051433244,52.9560891299428,
0.155347408007618));
#14656=CARTESIAN_POINT('Ctrl Pts',(2.30407741786964,51.8859408488594,-0.00343731121806405));
#14657=CARTESIAN_POINT('Ctrl Pts',(2.82987294110782,49.0837366230026,-0.162222030443749));
#14658=CARTESIAN_POINT('Ctrl Pts',(1.45900977058067,47.7841423687619,-0.268078509927538));
#14659=CARTESIAN_POINT('Ctrl Pts',(0.650199997975087,47.5679131979649,-0.321006749669432));
#14660=CARTESIAN_POINT('Ctrl Pts',(2.0543315503421,51.7564253212268,10.1070022498898));
#14661=CARTESIAN_POINT('Ctrl Pts',(2.6384447339141,51.0732410562991,10.0540740101479));
#14662=CARTESIAN_POINT('Ctrl Pts',(3.06100669698896,49.0897189524364,9.94821753066413));
#14663=CARTESIAN_POINT('Ctrl Pts',(0.891660702786476,46.9301690211716,9.78943281143844));
#14664=CARTESIAN_POINT('Ctrl Pts',(-2.09420984226096,47.5883285444086,9.63064809221277));
#14665=CARTESIAN_POINT('Ctrl Pts',(-3.16271070871609,50.4507453187398,9.47186337298707));
#14666=CARTESIAN_POINT('Ctrl Pts',(-1.33588428108549,52.9023161548447,9.3130786537614));
#14667=CARTESIAN_POINT('Ctrl Pts',(1.71396395726082,52.6959533505542,9.1542939345357));
#14668=CARTESIAN_POINT('Ctrl Pts',(3.19468533880467,50.0219503441049,8.99550921531003));
#14669=CARTESIAN_POINT('Ctrl Pts',(1.75073576944008,47.3276193341428,8.83672449608433));
#14670=CARTESIAN_POINT('Ctrl Pts',(-1.29598888724284,47.0799263820657,8.67793977685867));
#14671=CARTESIAN_POINT('Ctrl Pts',(-3.15625439074724,49.5054530852787,8.51915505763297));
#14672=CARTESIAN_POINT('Ctrl Pts',(-2.12702252124395,52.3837594017721,8.3603703384073));
#14673=CARTESIAN_POINT('Ctrl Pts',(0.849464028931752,53.0797581556832,8.2015856191816));
#14674=CARTESIAN_POINT('Ctrl Pts',(3.04827993961995,50.9562968815233,8.04280089995593));
#14675=CARTESIAN_POINT('Ctrl Pts',(2.45644609937722,47.9573577227543,7.88401618073025));
#14676=CARTESIAN_POINT('Ctrl Pts',(-0.384223656690181,46.8284257909833,
7.72523146150455));
#14677=CARTESIAN_POINT('Ctrl Pts',(-2.87314295645131,48.603016662361,7.56644674227888));
#14678=CARTESIAN_POINT('Ctrl Pts',(-2.73174736465177,51.65652320452,7.40766202305319));
#14679=CARTESIAN_POINT('Ctrl Pts',(-0.0894821750846268,53.1935098634703,
7.2488773038275));
#14680=CARTESIAN_POINT('Ctrl Pts',(2.63470246169916,51.806891124948,7.09009258460183));
#14681=CARTESIAN_POINT('Ctrl Pts',(2.94686052092051,48.7660933450191,6.93130786537613));
#14682=CARTESIAN_POINT('Ctrl Pts',(0.561216451468212,46.8549167573952,6.77252314615046));
#14683=CARTESIAN_POINT('Ctrl Pts',(-2.33821200770187,47.8230119075771,6.61373842692477));
#14684=CARTESIAN_POINT('Ctrl Pts',(-3.09704599956545,50.7841037026847,6.45495370769909));
#14685=CARTESIAN_POINT('Ctrl Pts',(-1.02058553931101,53.027361506501,6.2961689884734));
#14686=CARTESIAN_POINT('Ctrl Pts',(1.99020412284178,52.4991198628063,6.13738426924772));
#14687=CARTESIAN_POINT('Ctrl Pts',(3.17899478713483,49.6829752670549,5.97859955002203));
#14688=CARTESIAN_POINT('Ctrl Pts',(1.45746823818709,47.1570615778722,5.81981483079636));
#14689=CARTESIAN_POINT('Ctrl Pts',(-1.59834640661933,47.2338110508415,5.66103011157067));
#14690=CARTESIAN_POINT('Ctrl Pts',(-3.19090131955365,49.842960811716,5.50224539234499));
#14691=CARTESIAN_POINT('Ctrl Pts',(-1.86223878552621,52.5958773552336,5.3434606731193));
#14692=CARTESIAN_POINT('Ctrl Pts',(1.17127259398061,52.9723110618525,5.18467595389362));
#14693=CARTESIAN_POINT('Ctrl Pts',(3.13250326216747,50.6276430914849,5.02589123466794));
#14694=CARTESIAN_POINT('Ctrl Pts',(2.22597894024652,47.7083782390286,4.86710651544225));
#14695=CARTESIAN_POINT('Ctrl Pts',(-0.718392330115233,46.8870552530037,
4.70832179621657));
#14696=CARTESIAN_POINT('Ctrl Pts',(-3.00508728950221,48.9155817595572,4.54953707699089));
#14697=CARTESIAN_POINT('Ctrl Pts',(-2.54067447696744,51.9368752514998,4.3907523577652));
#14698=CARTESIAN_POINT('Ctrl Pts',(0.249683849399434,53.184991446354,4.23196763853952));
#14699=CARTESIAN_POINT('Ctrl Pts',(2.81146073613051,51.5173005854253,4.07318291931383));
#14700=CARTESIAN_POINT('Ctrl Pts',(2.79939176214431,48.4605461033315,3.91439820008815));
#14701=CARTESIAN_POINT('Ctrl Pts',(0.224525873257339,46.8131362326752,3.75561348086247));
#14702=CARTESIAN_POINT('Ctrl Pts',(-2.55588974295742,48.083247497474,3.59682876163679));
#14703=CARTESIAN_POINT('Ctrl Pts',(-2.9964305220077,51.108114013434,3.4380440424111));
#14704=CARTESIAN_POINT('Ctrl Pts',(-0.693788654191789,53.1185204586193,
3.27925932318542));
#14705=CARTESIAN_POINT('Ctrl Pts',(2.2440052606463,52.2739729326674,3.12047460395973));
#14706=CARTESIAN_POINT('Ctrl Pts',(3.12744943852504,49.3476407642752,2.96168988473405));
#14707=CARTESIAN_POINT('Ctrl Pts',(1.14776529852909,47.0185326735663,2.80290516550837));
#14708=CARTESIAN_POINT('Ctrl Pts',(-1.88267897290858,47.418908720578,2.64412044628268));
#14709=CARTESIAN_POINT('Ctrl Pts',(-3.18956182253859,50.1822310939418,2.485335727057));
#14710=CARTESIAN_POINT('Ctrl Pts',(-1.57645335916959,52.7787241137273,2.32655100783132));
#14711=CARTESIAN_POINT('Ctrl Pts',(1.47987180929927,52.8313407088695,2.16776628860563));
#14712=CARTESIAN_POINT('Ctrl Pts',(3.1813993829605,50.2919124492648,2.00898156937995));
#14713=CARTESIAN_POINT('Ctrl Pts',(1.97040718816538,47.4852415963503,1.85019685015426));
#14714=CARTESIAN_POINT('Ctrl Pts',(-1.04445788895881,46.9807936221355,1.69141213092858));
#14715=CARTESIAN_POINT('Ctrl Pts',(-3.10314366862385,49.2403730762436,1.5326274117029));
#14716=CARTESIAN_POINT('Ctrl Pts',(-2.32094349044031,52.1953905675652,1.37384269247722));
#14717=CARTESIAN_POINT('Ctrl Pts',(0.586023933536996,53.1405402527805,1.21505797325153));
#14718=CARTESIAN_POINT('Ctrl Pts',(2.95653208732984,51.2106247041231,1.05627325402585));
#14719=CARTESIAN_POINT('Ctrl Pts',(2.62031282301266,48.1723083024932,0.897488534800166));
#14720=CARTESIAN_POINT('Ctrl Pts',(-0.114618842478724,46.8073992676655,
0.73870381557448));
#14721=CARTESIAN_POINT('Ctrl Pts',(-2.74489717268617,48.3648959095816,0.579919096348797));
#14722=CARTESIAN_POINT('Ctrl Pts',(-2.86171691147896,51.4200305235974,0.421134377123114));
#14723=CARTESIAN_POINT('Ctrl Pts',(-0.359771596695991,53.1737105210381,
0.262349657897429));
#14724=CARTESIAN_POINT('Ctrl Pts',(2.47369900599749,52.0247800560049,0.103564938671747));
#14725=CARTESIAN_POINT('Ctrl Pts',(3.03820254789444,49.0162831390423,-0.0552197805539385));
#14726=CARTESIAN_POINT('Ctrl Pts',(1.56641916249631,47.6210153455288,-0.161076260037727));
#14727=CARTESIAN_POINT('Ctrl Pts',(0.698066426161006,47.3888678140614,-0.214004499779622));
#14728=CARTESIAN_POINT('Ctrl Pts',(2.19519710401913,51.8768634390787,10.2140044997796));
#14729=CARTESIAN_POINT('Ctrl Pts',(2.81936293975442,51.1468332160454,10.1610762600377));
#14730=CARTESIAN_POINT('Ctrl Pts',(3.27089998471491,49.0273009636042,10.0552197805539));
#14731=CARTESIAN_POINT('Ctrl Pts',(0.952801894221302,46.7196706522712,9.89643506132826));
#14732=CARTESIAN_POINT('Ctrl Pts',(-2.23780985117717,47.4229601865978,9.73765034210257));
#14733=CARTESIAN_POINT('Ctrl Pts',(-3.37957784247032,50.4816529338621,9.57886562287689));
#14734=CARTESIAN_POINT('Ctrl Pts',(-1.42748589177595,53.1013280290623,9.42008090365121));
#14735=CARTESIAN_POINT('Ctrl Pts',(1.83149049857389,52.8808149233369,9.26129618442552));
#14736=CARTESIAN_POINT('Ctrl Pts',(3.41374497355529,50.0234554796197,9.10251146519984));
#14737=CARTESIAN_POINT('Ctrl Pts',(1.8707837546172,47.1443741408005,8.94372674597414));
#14738=CARTESIAN_POINT('Ctrl Pts',(-1.38485487001487,46.8796968782645,8.78494202674848));
#14739=CARTESIAN_POINT('Ctrl Pts',(-3.37267881465492,49.4715419938827,8.62615730752278));
#14740=CARTESIAN_POINT('Ctrl Pts',(-2.27287249618527,52.5472138295189,8.46737258829712));
#14741=CARTESIAN_POINT('Ctrl Pts',(0.907711793633738,53.2909372312903,8.30858786907141));
#14742=CARTESIAN_POINT('Ctrl Pts',(3.25730055334983,51.0218701769695,8.14980314984575));
#14743=CARTESIAN_POINT('Ctrl Pts',(2.6248846553683,47.817293702757,7.99101843062005));
#14744=CARTESIAN_POINT('Ctrl Pts',(-0.410569880174145,46.610950886844,7.83223371139438));
#14745=CARTESIAN_POINT('Ctrl Pts',(-3.07015442389744,48.5072254881948,7.67344899216868));
#14746=CARTESIAN_POINT('Ctrl Pts',(-2.91906333366532,51.7701110323196,7.51466427294301));
#14747=CARTESIAN_POINT('Ctrl Pts',(-0.0956179695407002,53.4124888958548,
7.35587955371731));
#14748=CARTESIAN_POINT('Ctrl Pts',(2.81536405986217,51.9307896839258,7.19709483449164));
#14749=CARTESIAN_POINT('Ctrl Pts',(3.14892680317145,48.6814843421,7.03831011526595));
#14750=CARTESIAN_POINT('Ctrl Pts',(0.599699074273457,46.6392583393292,6.87952539604027));
#14751=CARTESIAN_POINT('Ctrl Pts',(-2.49854324976665,47.6737357924649,6.72074067681458));
#14752=CARTESIAN_POINT('Ctrl Pts',(-3.30941050295798,50.8378697085665,6.5619559575889));
#14753=CARTESIAN_POINT('Ctrl Pts',(-1.09056710925082,53.2349477428722,6.40317123836322));
#14754=CARTESIAN_POINT('Ctrl Pts',(2.12667245758927,52.6704845595713,6.24438651913753));
#14755=CARTESIAN_POINT('Ctrl Pts',(3.39697852045751,49.6612368750568,6.08560179991185));
#14756=CARTESIAN_POINT('Ctrl Pts',(1.55740686314017,46.9621212359219,5.92681708068617));
#14757=CARTESIAN_POINT('Ctrl Pts',(-1.7079450502748,47.04413342172,5.76803236146048));
#14758=CARTESIAN_POINT('Ctrl Pts',(-3.40970148403189,49.8321926315735,5.6092476422348));
#14759=CARTESIAN_POINT('Ctrl Pts',(-1.98993253464782,52.7738767151041,5.45046292300911));
#14760=CARTESIAN_POINT('Ctrl Pts',(1.2515867781396,53.1761224881817,5.29167820378343));
#14761=CARTESIAN_POINT('Ctrl Pts',(3.34729907073442,50.6706805902658,5.13289348455775));
#14762=CARTESIAN_POINT('Ctrl Pts',(2.37861435873046,47.5512416910727,4.97410876533206));
#14763=CARTESIAN_POINT('Ctrl Pts',(-0.767652505923838,46.6736005721958,
4.81532404610638));
#14764=CARTESIAN_POINT('Ctrl Pts',(-3.21114618238785,48.8412231800806,4.6565393268807));
#14765=CARTESIAN_POINT('Ctrl Pts',(-2.71488857441997,52.0696868245199,4.49775460765501));
#14766=CARTESIAN_POINT('Ctrl Pts',(0.266804675725645,53.403386370714,4.33896988842933));
#14767=CARTESIAN_POINT('Ctrl Pts',(3.00424265255014,51.6213419155723,4.18018516920365));
#14768=CARTESIAN_POINT('Ctrl Pts',(2.991346108787,48.3549857202091,4.02140044997796));
#14769=CARTESIAN_POINT('Ctrl Pts',(0.239921616678574,46.5946129232305,3.86261573075228));
#14770=CARTESIAN_POINT('Ctrl Pts',(-2.73114715148974,47.9518157417356,3.7038310115266));
#14771=CARTESIAN_POINT('Ctrl Pts',(-3.20189582018077,51.1840974125176,3.54504629230091));
#14772=CARTESIAN_POINT('Ctrl Pts',(-0.741361755472007,53.3323574660797,
3.38626157307523));
#14773=CARTESIAN_POINT('Ctrl Pts',(2.39787674426465,52.4298993001291,3.22747685384955));
#14774=CARTESIAN_POINT('Ctrl Pts',(3.34189870630822,49.3029084790112,3.06869213462386));
#14775=CARTESIAN_POINT('Ctrl Pts',(1.22646758698962,46.8140934019998,2.90990741539818));
#14776=CARTESIAN_POINT('Ctrl Pts',(-2.01177430606972,47.2419232422086,2.75112269617249));
#14777=CARTESIAN_POINT('Ctrl Pts',(-3.40827013768091,50.1947266835369,2.59233797694681));
#14778=CARTESIAN_POINT('Ctrl Pts',(-1.68455079614292,52.9692612793229,2.43355325772113));
#14779=CARTESIAN_POINT('Ctrl Pts',(1.58134664755177,53.0254857953999,2.27476853849544));
#14780=CARTESIAN_POINT('Ctrl Pts',(3.39954799946491,50.311928891491,2.11598381926976));
#14781=CARTESIAN_POINT('Ctrl Pts',(2.10551804672368,47.3128045645405,1.95719910004408));
#14782=CARTESIAN_POINT('Ctrl Pts',(-1.11607638637031,46.773766583091,1.79841438081839));
#14783=CARTESIAN_POINT('Ctrl Pts',(-3.31592628930028,49.1882854435608,1.63962966159271));
#14784=CARTESIAN_POINT('Ctrl Pts',(-2.48009062994636,52.3459285407497,1.48084494236703));
#14785=CARTESIAN_POINT('Ctrl Pts',(0.626207605861911,53.3558871579475,1.32206022314134));
#14786=CARTESIAN_POINT('Ctrl Pts',(3.15926154907436,51.2936372632267,1.16327550391566));
#14787=CARTESIAN_POINT('Ctrl Pts',(2.79998772337587,48.0469834478575,1.00449078468998));
#14788=CARTESIAN_POINT('Ctrl Pts',(-0.122478258698513,46.5884825744204,
0.845706065464291));
#14789=CARTESIAN_POINT('Ctrl Pts',(-2.93311482428801,48.2527767908454,0.686921346238607));
#14790=CARTESIAN_POINT('Ctrl Pts',(-3.05794489480291,51.5174020437455,0.528136627012925));
#14791=CARTESIAN_POINT('Ctrl Pts',(-0.384441141958736,53.3913319121335,
0.369351907787239));
#14792=CARTESIAN_POINT('Ctrl Pts',(2.64332059412533,52.1636192631504,0.210567188561558));
#14793=CARTESIAN_POINT('Ctrl Pts',(3.24653215468106,48.9488296550819,0.0517824693358721));
#14794=CARTESIAN_POINT('Ctrl Pts',(1.67382855441195,47.4578883222956,-0.0540740101479162));
#14795=CARTESIAN_POINT('Ctrl Pts',(0.745932854346925,47.2098224301578,-0.107002249889811));
#14796=CARTESIAN_POINT('Ctrl Pts',(2.33606265769616,51.9973015569306,10.3210067496694));
#14797=CARTESIAN_POINT('Ctrl Pts',(3.00028114559474,51.2204253757916,10.2680785099275));
#14798=CARTESIAN_POINT('Ctrl Pts',(3.48079327244086,48.9648829747721,10.1622220304438));
#14799=CARTESIAN_POINT('Ctrl Pts',(1.01394308565613,46.5091722833709,10.0034373112181));
#14800=CARTESIAN_POINT('Ctrl Pts',(-2.38140986009338,47.257591828787,9.84465259199239));
#14801=CARTESIAN_POINT('Ctrl Pts',(-3.59644497622454,50.5125605489844,9.6858678727667));
#14802=CARTESIAN_POINT('Ctrl Pts',(-1.5190875024664,53.3003399032799,9.52708315354102));
#14803=CARTESIAN_POINT('Ctrl Pts',(1.94901703988696,53.0656764961195,9.36829843431533));
#14804=CARTESIAN_POINT('Ctrl Pts',(3.63280460830591,50.0249606151346,9.20951371508965));
#14805=CARTESIAN_POINT('Ctrl Pts',(1.99083173979432,46.9611289474581,9.05072899586396));
#14806=CARTESIAN_POINT('Ctrl Pts',(-1.4737208527869,46.6794673744635,8.89194427663828));
#14807=CARTESIAN_POINT('Ctrl Pts',(-3.58910323856261,49.4376309024865,8.7331595574126));
#14808=CARTESIAN_POINT('Ctrl Pts',(-2.41872247112658,52.7106682572659,8.57437483818691));
#14809=CARTESIAN_POINT('Ctrl Pts',(0.965959558335722,53.5021163068972,8.41559011896124));
#14810=CARTESIAN_POINT('Ctrl Pts',(3.4663211670797,51.087443472416,8.25680539973554));
#14811=CARTESIAN_POINT('Ctrl Pts',(2.79332321135939,47.6772296827595,8.09802068050987));
#14812=CARTESIAN_POINT('Ctrl Pts',(-0.436916103658114,46.3934759827048,
7.93923596128417));
#14813=CARTESIAN_POINT('Ctrl Pts',(-3.26716589134357,48.4114343140284,7.7804512420585));
#14814=CARTESIAN_POINT('Ctrl Pts',(-3.10637930267888,51.8836988601192,7.62166652283282));
#14815=CARTESIAN_POINT('Ctrl Pts',(-0.101753763996771,53.6314679282393,
7.46288180360713));
#14816=CARTESIAN_POINT('Ctrl Pts',(2.99602565802517,52.0546882429035,7.30409708438145));
#14817=CARTESIAN_POINT('Ctrl Pts',(3.3509930854224,48.5968753391809,7.14531236515576));
#14818=CARTESIAN_POINT('Ctrl Pts',(0.638181697078704,46.4235999212631,6.98652764593008));
#14819=CARTESIAN_POINT('Ctrl Pts',(-2.65887449183142,47.5244596773528,6.8277429267044));
#14820=CARTESIAN_POINT('Ctrl Pts',(-3.52177500635052,50.8916357144483,6.66895820747871));
#14821=CARTESIAN_POINT('Ctrl Pts',(-1.16054867919063,53.4425339792431,6.51017348825302));
#14822=CARTESIAN_POINT('Ctrl Pts',(2.26314079233676,52.8418492563365,6.35138876902735));
#14823=CARTESIAN_POINT('Ctrl Pts',(3.6149622537802,49.6394984830586,6.19260404980166));
#14824=CARTESIAN_POINT('Ctrl Pts',(1.65734548809325,46.7671808939717,6.03381933057597));
#14825=CARTESIAN_POINT('Ctrl Pts',(-1.81754369393026,46.8544557925985,5.87503461135029));
#14826=CARTESIAN_POINT('Ctrl Pts',(-3.62850164851013,49.8214244514309,5.71624989212461));
#14827=CARTESIAN_POINT('Ctrl Pts',(-2.11762628376943,52.9518760749746,5.55746517289892));
#14828=CARTESIAN_POINT('Ctrl Pts',(1.3319009622986,53.3799339145109,5.39868045367324));
#14829=CARTESIAN_POINT('Ctrl Pts',(3.56209487930137,50.7137180890468,5.23989573444756));
#14830=CARTESIAN_POINT('Ctrl Pts',(2.53124977721441,47.3941051431169,5.08111101522187));
#14831=CARTESIAN_POINT('Ctrl Pts',(-0.816912681732443,46.460145891388,4.92232629599619));
#14832=CARTESIAN_POINT('Ctrl Pts',(-3.41720507527349,48.766864600604,4.76354157677051));
#14833=CARTESIAN_POINT('Ctrl Pts',(-2.88910267187251,52.2024983975401,4.60475685754483));
#14834=CARTESIAN_POINT('Ctrl Pts',(0.283925502051857,53.621781295074,4.44597213831914));
#14835=CARTESIAN_POINT('Ctrl Pts',(3.19702456896977,51.7253832457192,4.28718741909346));
#14836=CARTESIAN_POINT('Ctrl Pts',(3.18330045542969,48.2494253370868,4.12840269986777));
#14837=CARTESIAN_POINT('Ctrl Pts',(0.255317360099809,46.3760896137859,3.96961798064209));
#14838=CARTESIAN_POINT('Ctrl Pts',(-2.90640456002206,47.8203839859972,3.81083326141641));
#14839=CARTESIAN_POINT('Ctrl Pts',(-3.40736111835383,51.2600808116012,3.65204854219072));
#14840=CARTESIAN_POINT('Ctrl Pts',(-0.788934856752224,53.54619447354,3.49326382296504));
#14841=CARTESIAN_POINT('Ctrl Pts',(2.551748227883,52.5858256675908,3.33447910373936));
#14842=CARTESIAN_POINT('Ctrl Pts',(3.5563479740914,49.2581761937472,3.17569438451367));
#14843=CARTESIAN_POINT('Ctrl Pts',(1.30516987545015,46.6096541304332,3.01690966528799));
#14844=CARTESIAN_POINT('Ctrl Pts',(-2.14086963923087,47.0649377638391,2.8581249460623));
#14845=CARTESIAN_POINT('Ctrl Pts',(-3.62697845282322,50.2072222731319,2.69934022683662));
#14846=CARTESIAN_POINT('Ctrl Pts',(-1.79264823311626,53.1597984449186,2.54055550761094));
#14847=CARTESIAN_POINT('Ctrl Pts',(1.68282148580427,53.2196308819302,2.38177078838525));
#14848=CARTESIAN_POINT('Ctrl Pts',(3.61769661596932,50.3319453337173,2.22298606915957));
#14849=CARTESIAN_POINT('Ctrl Pts',(2.24062890528198,47.1403675327308,2.06420134993389));
#14850=CARTESIAN_POINT('Ctrl Pts',(-1.1876948837818,46.5667395440464,1.9054166307082));
#14851=CARTESIAN_POINT('Ctrl Pts',(-3.52870890997671,49.136197810878,1.74663191148252));
#14852=CARTESIAN_POINT('Ctrl Pts',(-2.63923776945242,52.4964665139341,1.58784719225684));
#14853=CARTESIAN_POINT('Ctrl Pts',(0.666391278186825,53.5712340631145,1.42906247303115));
#14854=CARTESIAN_POINT('Ctrl Pts',(3.36199101081887,51.3766498223304,1.27027775380547));
#14855=CARTESIAN_POINT('Ctrl Pts',(2.97966262373907,47.9216585932218,1.11149303457979));
#14856=CARTESIAN_POINT('Ctrl Pts',(-0.130337674918302,46.3695658811752,
0.952708315354101));
#14857=CARTESIAN_POINT('Ctrl Pts',(-3.12133247588985,48.1406576721092,0.793923596128419));
#14858=CARTESIAN_POINT('Ctrl Pts',(-3.25417287812687,51.6147735638935,0.635138876902735));
#14859=CARTESIAN_POINT('Ctrl Pts',(-0.409110687221481,53.6089533032289,
0.47635415767705));
#14860=CARTESIAN_POINT('Ctrl Pts',(2.81294218225317,52.3024584702958,0.317569438451368));
#14861=CARTESIAN_POINT('Ctrl Pts',(3.45486176146768,48.8813761711215,0.158784719225683));
#14862=CARTESIAN_POINT('Ctrl Pts',(1.78123794632758,47.2947612990625,0.0529282397418946));
#14863=CARTESIAN_POINT('Ctrl Pts',(0.793799282532844,47.0307770462543,0.));
#14864=CARTESIAN_POINT('Ctrl Pts',(0.793799282532844,47.0307770462543,0.));
#14865=CARTESIAN_POINT('Ctrl Pts',(0.886857327319536,47.0648180947248,2.20021361319926E-16));
#14866=CARTESIAN_POINT('Ctrl Pts',(0.97784812376529,47.1036280421655,1.56093797443782E-15));
#14867=CARTESIAN_POINT('Ctrl Pts',(1.06656383114865,47.146878310404,8.32667268468867E-16));
#14868=CARTESIAN_POINT('Ctrl Pts',(1.15724741706422,47.191087949614,8.82421707898277E-17));
#14869=CARTESIAN_POINT('Ctrl Pts',(1.24555453014161,47.2399377005581,4.94586033878426E-16));
#14870=CARTESIAN_POINT('Ctrl Pts',(1.33123425142126,47.2931221802054,2.77555756156289E-16));
#14871=CARTESIAN_POINT('Ctrl Pts',(1.414183141195,47.3446115346763,6.74427875860411E-17));
#14872=CARTESIAN_POINT('Ctrl Pts',(1.49466977869018,47.4001645661104,-2.35200004845136E-15));
#14873=CARTESIAN_POINT('Ctrl Pts',(1.57243277080527,47.4595348565004,-3.10862446895044E-15));
#14874=CARTESIAN_POINT('Ctrl Pts',(1.64047538890598,47.5114838605917,-3.77067083688713E-15));
#14875=CARTESIAN_POINT('Ctrl Pts',(1.70643241927354,47.5663561703348,-2.05196266536534E-15));
#14876=CARTESIAN_POINT('Ctrl Pts',(1.77010348490124,47.6239996814536,-3.66373598126302E-15));
#14877=CARTESIAN_POINT('Ctrl Pts',(1.78344332214389,47.6360766751216,-4.00142145101522E-15));
#14878=CARTESIAN_POINT('Ctrl Pts',(1.79668458295983,47.648277209747,-1.16810055785692E-16));
#14879=CARTESIAN_POINT('Ctrl Pts',(1.80980825419109,47.6605835920549,-1.11022302462516E-16));
#14880=CARTESIAN_POINT('Ctrl Pts',(1.88223649041001,47.7285012919949,-7.90802675333328E-17));
#14881=CARTESIAN_POINT('Ctrl Pts',(1.95119902453439,47.7997400265197,-4.2204114024801E-15));
#14882=CARTESIAN_POINT('Ctrl Pts',(2.01645648006057,47.87400881514,-3.58046925441613E-15));
#14883=CARTESIAN_POINT('Ctrl Pts',(2.08135180887242,47.9478654713505,-2.94407827373316E-15));
#14884=CARTESIAN_POINT('Ctrl Pts',(2.14258355052389,48.0247194439553,-4.09959586981255E-15));
#14885=CARTESIAN_POINT('Ctrl Pts',(2.19987267902198,48.1043113151144,-3.33066907387547E-15));
#14886=CARTESIAN_POINT('Ctrl Pts',(2.25572844020942,48.1819118069438,-2.58098073665603E-15));
#14887=CARTESIAN_POINT('Ctrl Pts',(2.30783667769722,48.2621156470778,4.07626245988852E-17));
#14888=CARTESIAN_POINT('Ctrl Pts',(2.35589192627243,48.3446965327013,-4.71844785465692E-16));
#14889=CARTESIAN_POINT('Ctrl Pts',(2.37661944628707,48.3803158877216,-6.92946135823573E-16));
#14890=CARTESIAN_POINT('Ctrl Pts',(2.39659231188801,48.4163775922232,-5.2526661233185E-16));
#14891=CARTESIAN_POINT('Ctrl Pts',(2.41578302796428,48.4528638195851,-3.60822483003176E-16));
#14892=CARTESIAN_POINT('Ctrl Pts',(2.42944452020578,48.4788376451601,-2.43757950963101E-16));
#14893=CARTESIAN_POINT('Ctrl Pts',(2.44270960171289,48.5050266109815,-2.2454156296485E-15));
#14894=CARTESIAN_POINT('Ctrl Pts',(2.45556775734007,48.5314242897153,-2.44249065417534E-15));
#14895=CARTESIAN_POINT('Ctrl Pts',(2.46118164896502,48.5429495591131,-2.52853392987966E-15));
#14896=CARTESIAN_POINT('Ctrl Pts',(2.46671705248137,48.5545128335615,1.92714193980372E-16));
#14897=CARTESIAN_POINT('Ctrl Pts',(2.47216939081917,48.566105287244,1.94289029309402E-16));
#14898=CARTESIAN_POINT('Ctrl Pts',(2.51239835158546,48.6516378304363,2.05908628963686E-16));
#14899=CARTESIAN_POINT('Ctrl Pts',(2.54817131413657,48.7388840438779,-2.2713001230117E-15));
#14900=CARTESIAN_POINT('Ctrl Pts',(2.57923728625574,48.8276067891984,-1.83186799063151E-15));
#14901=CARTESIAN_POINT('Ctrl Pts',(2.60961659647764,48.9143684650762,-1.4021487782457E-15));
#14902=CARTESIAN_POINT('Ctrl Pts',(2.63549491455905,49.0025427959324,5.44463455921423E-16));
#14903=CARTESIAN_POINT('Ctrl Pts',(2.65658840962129,49.0919168481172,1.47104550762833E-15));
#14904=CARTESIAN_POINT('Ctrl Pts',(2.66032086411668,49.107731419475,1.63500246848459E-15));
#14905=CARTESIAN_POINT('Ctrl Pts',(2.66390337128728,49.1235835631294,1.68482728082412E-15));
#14906=CARTESIAN_POINT('Ctrl Pts',(2.66733418587856,49.1394721050097,1.9151347174784E-15));
#14907=CARTESIAN_POINT('Ctrl Pts',(2.68744489614248,49.2326073805454,3.26407681196226E-15));
#14908=CARTESIAN_POINT('Ctrl Pts',(2.70234744457541,49.3269943616445,-3.40775973016887E-15));
#14909=CARTESIAN_POINT('Ctrl Pts',(2.71212035484507,49.4222239812899,-3.05311331771918E-15));
#14910=CARTESIAN_POINT('Ctrl Pts',(2.71539798866634,49.4541620441108,-2.93417217900389E-15));
#14911=CARTESIAN_POINT('Ctrl Pts',(2.7180982270661,49.4861947652343,9.25563036540978E-16));
#14912=CARTESIAN_POINT('Ctrl Pts',(2.72022280748871,49.5183062439642,7.7715611723761E-16));
#14913=CARTESIAN_POINT('Ctrl Pts',(2.7214113229284,49.5362697853089,6.94135529703041E-16));
#14914=CARTESIAN_POINT('Ctrl Pts',(2.72241968039311,49.5542579679131,3.13605320939017E-15));
#14915=CARTESIAN_POINT('Ctrl Pts',(2.72324810469235,49.5722679631563,3.27515792264421E-15));
#14916=CARTESIAN_POINT('Ctrl Pts',(2.72382227638594,49.584750491107,3.37156985656304E-15));
#14917=CARTESIAN_POINT('Ctrl Pts',(2.72430989801868,49.597241968614,5.36242468914633E-16));
#14918=CARTESIAN_POINT('Ctrl Pts',(2.72471091953202,49.6097319728608,4.9960036108132E-16));
#14919=CARTESIAN_POINT('Ctrl Pts',(2.72770312507896,49.7029256264329,2.26196778816368E-16));
#14920=CARTESIAN_POINT('Ctrl Pts',(2.72588562145581,49.7961843599269,5.65648183417809E-16));
#14921=CARTESIAN_POINT('Ctrl Pts',(2.71939754410297,49.8891328761941,1.23512311489549E-15));
#14922=CARTESIAN_POINT('Ctrl Pts',(2.71289651492916,49.9822669408875,1.90593448534879E-15));
#14923=CARTESIAN_POINT('Ctrl Pts',(2.70170586262138,50.075090530546,4.03808733020254E-15));
#14924=CARTESIAN_POINT('Ctrl Pts',(2.68591451135734,50.1672140980482,5.39845945723982E-15));
#14925=CARTESIAN_POINT('Ctrl Pts',(2.67034644847316,50.2580350460475,6.7395960367198E-15));
#14926=CARTESIAN_POINT('Ctrl Pts',(2.65030640580631,50.348176475764,4.44579026743949E-15));
#14927=CARTESIAN_POINT('Ctrl Pts',(2.6258365433358,50.4372399806273,4.7045700668491E-15));
#14928=CARTESIAN_POINT('Ctrl Pts',(2.61632310862035,50.4718662414028,4.80517891703474E-15));
#14929=CARTESIAN_POINT('Ctrl Pts',(2.60613967316216,50.5063292337113,2.00838248105005E-15));
#14930=CARTESIAN_POINT('Ctrl Pts',(2.59528714815,50.5406040828628,1.99840144432528E-15));
#14931=CARTESIAN_POINT('Ctrl Pts',(2.5894827385199,50.5589357857857,1.99306314511668E-15));
#14932=CARTESIAN_POINT('Ctrl Pts',(2.58348691601437,50.5772136532266,4.83308587950495E-15));
#14933=CARTESIAN_POINT('Ctrl Pts',(2.5772997243422,50.5954337650825,4.94049245958195E-15));
#14934=CARTESIAN_POINT('Ctrl Pts',(2.5718499055314,50.6114824530153,5.03509861234435E-15));
#14935=CARTESIAN_POINT('Ctrl Pts',(2.5662511329767,50.6274874088124,-7.84775819580116E-16));
#14936=CARTESIAN_POINT('Ctrl Pts',(2.56050956139753,50.6434295339054,-4.85722573273506E-16));
#14937=CARTESIAN_POINT('Ctrl Pts',(2.5280829941685,50.7334655778652,1.20323489468014E-15));
#14938=CARTESIAN_POINT('Ctrl Pts',(2.49106539149493,50.821622868814,6.21849611564327E-15));
#14939=CARTESIAN_POINT('Ctrl Pts',(2.4495298227146,50.9074566537128,7.32747196252603E-15));
#14940=CARTESIAN_POINT('Ctrl Pts',(2.41837814612936,50.971831992387,8.15920384768811E-15));
#14941=CARTESIAN_POINT('Ctrl Pts',(2.3846839652608,51.0348998219571,5.7554240688827E-15));
#14942=CARTESIAN_POINT('Ctrl Pts',(2.34846073836671,51.0964553528622,5.51642065360625E-15));
#14943=CARTESIAN_POINT('Ctrl Pts',(2.33352951737538,51.1218285543683,5.41790340052968E-15));
#14944=CARTESIAN_POINT('Ctrl Pts',(2.31816842560509,51.1469446029168,3.64806198334203E-15));
#14945=CARTESIAN_POINT('Ctrl Pts',(2.30237774790741,51.1717882500971,3.51801920928096E-15));
#14946=CARTESIAN_POINT('Ctrl Pts',(2.29294436447259,51.1866298961782,3.44033138776168E-15));
#14947=CARTESIAN_POINT('Ctrl Pts',(2.28336234355129,51.2013669072614,6.3072103585326E-15));
#14948=CARTESIAN_POINT('Ctrl Pts',(2.27363372765336,51.2159939545931,6.13398221105399E-15));
#14949=CARTESIAN_POINT('Ctrl Pts',(2.22610568566997,51.2874527239563,5.28769587880953E-15));
#14950=CARTESIAN_POINT('Ctrl Pts',(2.17506913351012,51.3563092996365,3.87680889073946E-15));
#14951=CARTESIAN_POINT('Ctrl Pts',(2.12055847790166,51.4222108593004,3.96210841913103E-15));
#14952=CARTESIAN_POINT('Ctrl Pts',(2.06897016170881,51.4845794083408,4.04283500355103E-15));
#14953=CARTESIAN_POINT('Ctrl Pts',(2.01426976271456,51.5443015075236,-7.75360004353403E-16));
#14954=CARTESIAN_POINT('Ctrl Pts',(1.95646265307235,51.601042205567,1.35308431126191E-16));
#14955=CARTESIAN_POINT('Ctrl Pts',(1.94349660304568,51.613769061034,3.33958961373067E-16));
#14956=CARTESIAN_POINT('Ctrl Pts',(1.93037416921141,51.6263457638983,-1.91541932274788E-17));
#14957=CARTESIAN_POINT('Ctrl Pts',(1.91709858156531,51.6387709851531,5.55111512312578E-17));
#14958=CARTESIAN_POINT('Ctrl Pts',(1.91346599666507,51.6359872033749,10.));
#14959=CARTESIAN_POINT('Ctrl Pts',(1.97508237614856,51.5780829367082,10.));
#14960=CARTESIAN_POINT('Ctrl Pts',(2.03332776396516,51.5170283993854,10.));
#14961=CARTESIAN_POINT('Ctrl Pts',(2.08820515281575,51.4532083325515,10.));
#14962=CARTESIAN_POINT('Ctrl Pts',(2.14453492336427,51.3876992076378,10.));
#14963=CARTESIAN_POINT('Ctrl Pts',(2.19731649744598,51.3192757995672,10.));
#14964=CARTESIAN_POINT('Ctrl Pts',(2.24652756554328,51.2483056584003,10.));
#14965=CARTESIAN_POINT('Ctrl Pts',(2.29742972651859,51.1748966939174,10.));
#14966=CARTESIAN_POINT('Ctrl Pts',(2.3445123533709,51.0987624345107,10.));
#14967=CARTESIAN_POINT('Ctrl Pts',(2.38771583441218,51.0202656546028,10.));
#14968=CARTESIAN_POINT('Ctrl Pts',(2.40661735736774,50.985923313393,10.));
#14969=CARTESIAN_POINT('Ctrl Pts',(2.42477589363752,50.9511282648287,10.));
#14970=CARTESIAN_POINT('Ctrl Pts',(2.44218400642212,50.915908799321,10.));
#14971=CARTESIAN_POINT('Ctrl Pts',(2.45169083165477,50.8966749336221,10.));
#14972=CARTESIAN_POINT('Ctrl Pts',(2.46097382245344,50.8773144696349,10.));
#14973=CARTESIAN_POINT('Ctrl Pts',(2.47003156402945,50.8578318865754,10.));
#14974=CARTESIAN_POINT('Ctrl Pts',(2.47868023930483,50.8392291771701,10.));
#14975=CARTESIAN_POINT('Ctrl Pts',(2.48712604040155,50.8205091346798,10.));
#14976=CARTESIAN_POINT('Ctrl Pts',(2.49535364052389,50.8017084231113,10.));
#14977=CARTESIAN_POINT('Ctrl Pts',(2.53191898243085,50.7181537490415,10.));
#14978=CARTESIAN_POINT('Ctrl Pts',(2.56422392604051,50.6329156432926,10.));
#14979=CARTESIAN_POINT('Ctrl Pts',(2.59224406717849,50.546392863989,10.));
#14980=CARTESIAN_POINT('Ctrl Pts',(2.62072600083341,50.4584441256999,10.));
#14981=CARTESIAN_POINT('Ctrl Pts',(2.64478122692469,50.3691672645249,10.));
#14982=CARTESIAN_POINT('Ctrl Pts',(2.6643450084389,50.2789439546436,10.));
#14983=CARTESIAN_POINT('Ctrl Pts',(2.68356990503497,50.1902834979848,10.));
#14984=CARTESIAN_POINT('Ctrl Pts',(2.69845787026654,50.1007081883537,10.));
#14985=CARTESIAN_POINT('Ctrl Pts',(2.70890477495091,50.0105573646828,10.));
#14986=CARTESIAN_POINT('Ctrl Pts',(2.71303564023117,49.9749103554738,10.));
#14987=CARTESIAN_POINT('Ctrl Pts',(2.7164716351295,49.9391731818997,10.));
#14988=CARTESIAN_POINT('Ctrl Pts',(2.7192042931916,49.9033662888073,10.));
#14989=CARTESIAN_POINT('Ctrl Pts',(2.72082178426693,49.8821717856182,10.));
#14990=CARTESIAN_POINT('Ctrl Pts',(2.72219283242366,49.8609528514772,10.));
#14991=CARTESIAN_POINT('Ctrl Pts',(2.72331547946922,49.8397137034055,10.));
#14992=CARTESIAN_POINT('Ctrl Pts',(2.72406272622749,49.825576682685,10.));
#14993=CARTESIAN_POINT('Ctrl Pts',(2.72469984227435,49.8114307112021,10.));
#14994=CARTESIAN_POINT('Ctrl Pts',(2.72522589886129,49.7972915862557,10.));
#14995=CARTESIAN_POINT('Ctrl Pts',(2.72876702640459,49.7021146679759,10.));
#14996=CARTESIAN_POINT('Ctrl Pts',(2.72728895308013,49.6070864076313,10.));
#14997=CARTESIAN_POINT('Ctrl Pts',(2.72073289392688,49.5126053984232,10.));
#14998=CARTESIAN_POINT('Ctrl Pts',(2.71419948325485,49.4184507821463,10.));
#14999=CARTESIAN_POINT('Ctrl Pts',(2.70262347017024,49.3248386892842,10.));
#15000=CARTESIAN_POINT('Ctrl Pts',(2.68589868103377,49.2321456940246,10.));
#15001=CARTESIAN_POINT('Ctrl Pts',(2.68396182243872,49.221411135693,10.));
#15002=CARTESIAN_POINT('Ctrl Pts',(2.68195585483714,49.2106888933147,10.));
#15003=CARTESIAN_POINT('Ctrl Pts',(2.67988056808785,49.199979545295,10.));
#15004=CARTESIAN_POINT('Ctrl Pts',(2.66233627408987,49.1094436469436,10.));
#15005=CARTESIAN_POINT('Ctrl Pts',(2.63984221727701,49.0198289846102,10.));
#15006=CARTESIAN_POINT('Ctrl Pts',(2.61267377634981,48.9313735730564,10.));
#15007=CARTESIAN_POINT('Ctrl Pts',(2.60192598368317,48.8963807508268,10.));
#15008=CARTESIAN_POINT('Ctrl Pts',(2.5904460787386,48.8615693998425,10.));
#15009=CARTESIAN_POINT('Ctrl Pts',(2.57824891659478,48.8269545976856,10.));
#15010=CARTESIAN_POINT('Ctrl Pts',(2.57231002899096,48.8101003969286,10.));
#15011=CARTESIAN_POINT('Ctrl Pts',(2.56620107697497,48.7932927979567,10.));
#15012=CARTESIAN_POINT('Ctrl Pts',(2.55992367518301,48.7765335691397,10.));
#15013=CARTESIAN_POINT('Ctrl Pts',(2.55466427682359,48.7624921769418,10.));
#15014=CARTESIAN_POINT('Ctrl Pts',(2.5492894967777,48.7484924666187,10.));
#15015=CARTESIAN_POINT('Ctrl Pts',(2.54380264072253,48.734540236572,10.));
#15016=CARTESIAN_POINT('Ctrl Pts',(2.50957844436993,48.6475133753102,10.));
#15017=CARTESIAN_POINT('Ctrl Pts',(2.47097567284871,48.562274017746,10.));
#15018=CARTESIAN_POINT('Ctrl Pts',(2.42832689037754,48.4790541200089,10.));
#15019=CARTESIAN_POINT('Ctrl Pts',(2.38409691699032,48.3927488693328,10.));
#15020=CARTESIAN_POINT('Ctrl Pts',(2.33551523257715,48.308614870025,10.));
#15021=CARTESIAN_POINT('Ctrl Pts',(2.2828968139237,48.2269143645578,10.));
#15022=CARTESIAN_POINT('Ctrl Pts',(2.22970003533411,48.1443158408617,10.));
#15023=CARTESIAN_POINT('Ctrl Pts',(2.17237687628308,48.0642037829466,10.));
#15024=CARTESIAN_POINT('Ctrl Pts',(2.11120119278049,47.9868645265092,10.));
#15025=CARTESIAN_POINT('Ctrl Pts',(2.08739174172464,47.9567642458843,10.));
#15026=CARTESIAN_POINT('Ctrl Pts',(2.06299821502567,47.9270842051726,10.));
#15027=CARTESIAN_POINT('Ctrl Pts',(2.03803489359285,47.8978423233543,10.));
#15028=CARTESIAN_POINT('Ctrl Pts',(2.01823053305732,47.8746436167309,10.));
#15029=CARTESIAN_POINT('Ctrl Pts',(1.9980675313089,47.8517206920118,10.));
#15030=CARTESIAN_POINT('Ctrl Pts',(1.97755259625766,47.8290828275254,10.));
#15031=CARTESIAN_POINT('Ctrl Pts',(1.9658214299723,47.8161376950172,10.));
#15032=CARTESIAN_POINT('Ctrl Pts',(1.95397995403824,47.8032911219115,10.));
#15033=CARTESIAN_POINT('Ctrl Pts',(1.94203528977052,47.7905504717426,10.));
#15034=CARTESIAN_POINT('Ctrl Pts',(1.87297907510553,47.716892388659,10.));
#15035=CARTESIAN_POINT('Ctrl Pts',(1.80042221874533,47.6467115453198,10.));
#15036=CARTESIAN_POINT('Ctrl Pts',(1.72467678835325,47.5802968989121,10.));
#15037=CARTESIAN_POINT('Ctrl Pts',(1.66041809926708,47.5239539869742,10.));
#15038=CARTESIAN_POINT('Ctrl Pts',(1.59386353521053,47.4703215800399,10.));
#15039=CARTESIAN_POINT('Ctrl Pts',(1.52517876205432,47.4195910301052,10.));
#15040=CARTESIAN_POINT('Ctrl Pts',(1.50256045600412,47.4028851570014,10.));
#15041=CARTESIAN_POINT('Ctrl Pts',(1.47971097867339,47.3864941045494,10.));
#15042=CARTESIAN_POINT('Ctrl Pts',(1.45663577987822,47.370425142175,10.));
#15043=CARTESIAN_POINT('Ctrl Pts',(1.43994825627114,47.3588043890302,10.));
#15044=CARTESIAN_POINT('Ctrl Pts',(1.4231416418667,47.3473515143883,10.));
#15045=CARTESIAN_POINT('Ctrl Pts',(1.40623277255848,47.3360788992253,10.));
#15046=CARTESIAN_POINT('Ctrl Pts',(1.31987534930084,47.2785071017792,10.));
#15047=CARTESIAN_POINT('Ctrl Pts',(1.23076881304987,47.2255738593114,10.));
#15048=CARTESIAN_POINT('Ctrl Pts',(1.1392218397819,47.1776007658582,10.));
#15049=CARTESIAN_POINT('Ctrl Pts',(1.04767486651393,47.129627672405,10.));
#15050=CARTESIAN_POINT('Ctrl Pts',(0.95368681063774,47.0866138170145,10.));
#15051=CARTESIAN_POINT('Ctrl Pts',(0.857528305927518,47.0489215422574,10.));
#15052=CARTESIAN_POINT('Ctrl Pts',(0.836959977015811,47.0408591549837,10.));
#15053=CARTESIAN_POINT('Ctrl Pts',(0.816292224819087,47.0330404248373,10.));
#15054=CARTESIAN_POINT('Ctrl Pts',(0.795528952796256,47.0254641741959,10.));
#15055=CARTESIAN_POINT('Ctrl Pts',(-2.51945660451951,49.9980217824357,8.38741669750802));
#15056=CARTESIAN_POINT('Ctrl Pts',(-2.52057809732048,49.8678907140886,8.3956620675864));
#15057=CARTESIAN_POINT('Ctrl Pts',(-2.51136663771178,49.7379189147974,8.40390743766478));
#15058=CARTESIAN_POINT('Ctrl Pts',(-2.49126921968861,49.6096529277652,8.41215280774316));
#15059=CARTESIAN_POINT('Ctrl Pts',(-2.36226094604997,48.7862947464054,8.46508104748506));
#15060=CARTESIAN_POINT('Ctrl Pts',(-1.78469192526039,48.0332253161362,8.51800928722695));
#15061=CARTESIAN_POINT('Ctrl Pts',(-1.0229389667433,47.6951420412712,8.57093752696885));
#15062=CARTESIAN_POINT('Ctrl Pts',(-0.261186008226218,47.3570587664063,
8.62386576671074));
#15063=CARTESIAN_POINT('Ctrl Pts',(0.684750888018369,47.4339616469457,8.67679400645263));
#15064=CARTESIAN_POINT('Ctrl Pts',(1.38187565610585,47.8906765340663,8.72972224619453));
#15065=CARTESIAN_POINT('Ctrl Pts',(2.07900042419332,48.3473914211868,8.78265048593643));
#15066=CARTESIAN_POINT('Ctrl Pts',(2.52731306412369,49.1839183148884,8.83557872567832));
#15067=CARTESIAN_POINT('Ctrl Pts',(2.52160466940449,50.0172895232695,8.88850696542022));
#15068=CARTESIAN_POINT('Ctrl Pts',(2.51589627468529,50.8506607316505,8.94143520516211));
#15069=CARTESIAN_POINT('Ctrl Pts',(2.05616684531652,51.680876254711,8.994363444904));
#15070=CARTESIAN_POINT('Ctrl Pts',(1.35284878290834,52.1280194333839,9.0472916846459));
#15071=CARTESIAN_POINT('Ctrl Pts',(0.649530720500157,52.5751626120567,9.10021992438779));
#15072=CARTESIAN_POINT('Ctrl Pts',(-0.297375974947443,52.6392334463419,
9.15314816412969));
#15073=CARTESIAN_POINT('Ctrl Pts',(-1.05442280676571,52.2906911006495,9.20607640387158));
#15074=CARTESIAN_POINT('Ctrl Pts',(-1.81146963858398,51.9421487549572,9.25900464361348));
#15075=CARTESIAN_POINT('Ctrl Pts',(-2.37865660677292,51.1809932292873,9.31193288335537));
#15076=CARTESIAN_POINT('Ctrl Pts',(-2.49637780059787,50.3560586662194,9.36486112309726));
#15077=CARTESIAN_POINT('Ctrl Pts',(-2.51310024819857,50.2388756462662,9.37237964790085));
#15078=CARTESIAN_POINT('Ctrl Pts',(-2.52075311949145,50.1204056565824,9.37989817270443));
#15079=CARTESIAN_POINT('Ctrl Pts',(-2.51977158007336,50.0018123497868,9.38741669750802));
#15080=CARTESIAN_POINT('Ctrl Pts',(-0.79379928253289,47.0307770462543,10.));
#15081=CARTESIAN_POINT('Ctrl Pts',(-1.78123794632762,47.2947612990625,9.94707176025811));
#15082=CARTESIAN_POINT('Ctrl Pts',(-3.45486289525881,48.881369057802,9.84121528077431));
#15083=CARTESIAN_POINT('Ctrl Pts',(-2.81294119083295,52.3024617009106,9.68243056154864));
#15084=CARTESIAN_POINT('Ctrl Pts',(0.409110549274297,53.6089507129763,9.52364584232294));
#15085=CARTESIAN_POINT('Ctrl Pts',(3.25417230454442,51.6147744981929,9.36486112309727));
#15086=CARTESIAN_POINT('Ctrl Pts',(3.12133210059845,48.1406572795451,9.20607640387158));
#15087=CARTESIAN_POINT('Ctrl Pts',(0.130337574092825,46.3695668156037,9.0472916846459));
#15088=CARTESIAN_POINT('Ctrl Pts',(-2.97966211384112,47.921658696003,8.88850696542022));
#15089=CARTESIAN_POINT('Ctrl Pts',(-3.36199053548259,51.3766497311158,8.72972224619453));
#15090=CARTESIAN_POINT('Ctrl Pts',(-0.666391154437672,53.5712334545473,
8.57093752696884));
#15091=CARTESIAN_POINT('Ctrl Pts',(2.63923735448624,52.496466169517,8.41215280774317));
#15092=CARTESIAN_POINT('Ctrl Pts',(3.52870838065631,49.1361979230418,8.25336808851748));
#15093=CARTESIAN_POINT('Ctrl Pts',(1.18769469860156,46.5667400770053,8.0945833692918));
#15094=CARTESIAN_POINT('Ctrl Pts',(-2.24062856177748,47.1403679623332,7.93579865006611));
#15095=CARTESIAN_POINT('Ctrl Pts',(-3.61769606676686,50.3319452862105,7.77701393084044));
#15096=CARTESIAN_POINT('Ctrl Pts',(-1.68282122891848,53.2196303903089,7.61822921161475));
#15097=CARTESIAN_POINT('Ctrl Pts',(1.79264795986253,53.1597979648733,7.45944449238905));
#15098=CARTESIAN_POINT('Ctrl Pts',(3.62697790104741,50.2072222411372,7.30065977316339));
#15099=CARTESIAN_POINT('Ctrl Pts',(2.14086931327707,47.0649382107817,7.14187505393769));
#15100=CARTESIAN_POINT('Ctrl Pts',(-1.30516967674285,46.6096546462972,6.98309033471202));
#15101=CARTESIAN_POINT('Ctrl Pts',(-3.556347432871,49.2581763067165,6.82430561548633));
#15102=CARTESIAN_POINT('Ctrl Pts',(-2.55174783950134,52.5858252740066,6.66552089626065));
#15103=CARTESIAN_POINT('Ctrl Pts',(0.788934736670248,53.5461939338473,6.50673617703496));
#15104=CARTESIAN_POINT('Ctrl Pts',(3.40736059977763,51.2600806198138,6.34795145780928));
#15105=CARTESIAN_POINT('Ctrl Pts',(2.90640411768017,47.8203843177281,6.1891667385836));
#15106=CARTESIAN_POINT('Ctrl Pts',(-0.255317321240407,46.3760901653225,
6.03038201935791));
#15107=CARTESIAN_POINT('Ctrl Pts',(-3.18329997094959,48.2494256035161,5.87159730013223));
#15108=CARTESIAN_POINT('Ctrl Pts',(-3.19702408239961,51.7253829831247,5.71281258090654));
#15109=CARTESIAN_POINT('Ctrl Pts',(-0.283925458840122,53.6217807438589,
5.55402786168086));
#15110=CARTESIAN_POINT('Ctrl Pts',(2.889102232167,52.2024980623317,5.39524314245518));
#15111=CARTESIAN_POINT('Ctrl Pts',(3.41720455519345,48.7668647882805,5.23645842322949));
#15112=CARTESIAN_POINT('Ctrl Pts',(0.816912557402795,46.4601464301344,5.07767370400381));
#15113=CARTESIAN_POINT('Ctrl Pts',(-2.53124939197203,47.3941055397199,4.91888898477813));
#15114=CARTESIAN_POINT('Ctrl Pts',(-3.56209433716996,50.7137179804228,4.76010426555244));
#15115=CARTESIAN_POINT('Ctrl Pts',(-1.33190075959052,53.3799334001034,4.60131954632676));
#15116=CARTESIAN_POINT('Ctrl Pts',(2.1176259614783,52.951875625715,4.44253482710107));
#15117=CARTESIAN_POINT('Ctrl Pts',(3.62850109627196,49.8214244786094,4.28375010787539));
#15118=CARTESIAN_POINT('Ctrl Pts',(1.81754341731002,46.8544562713326,4.12496538864971));
#15119=CARTESIAN_POINT('Ctrl Pts',(-1.65734523585442,46.76718138599,3.96618066942402));
#15120=CARTESIAN_POINT('Ctrl Pts',(-3.61496170360255,49.6394985379234,3.80739595019834));
#15121=CARTESIAN_POINT('Ctrl Pts',(-2.26314044789927,52.8418488238258,3.64861123097266));
#15122=CARTESIAN_POINT('Ctrl Pts',(1.160548502562,53.4425334553022,3.48982651174698));
#15123=CARTESIAN_POINT('Ctrl Pts',(3.52177447035456,50.8916355787576,3.33104179252129));
#15124=CARTESIAN_POINT('Ctrl Pts',(2.65887408716728,47.524460054095,3.17225707329561));
#15125=CARTESIAN_POINT('Ctrl Pts',(-0.638181599955106,46.4236004656121,
3.01347235406992));
#15126=CARTESIAN_POINT('Ctrl Pts',(-3.35099257541117,48.5968755526526,2.85468763484424));
#15127=CARTESIAN_POINT('Ctrl Pts',(-2.9960252020633,52.054687930335,2.69590291561856));
#15128=CARTESIAN_POINT('Ctrl Pts',(0.101753748544503,53.6314673752793,2.53711819639287));
#15129=CARTESIAN_POINT('Ctrl Pts',(3.10637882983628,51.8836985739372,2.37833347716719));
#15130=CARTESIAN_POINT('Ctrl Pts',(3.26716539423699,48.4114345548525,2.2195487579415));
#15131=CARTESIAN_POINT('Ctrl Pts',(0.436916036883408,46.3934765333616,2.06076403871582));
#15132=CARTESIAN_POINT('Ctrl Pts',(-2.79332278567043,47.6772300330011,1.90197931949014));
#15133=CARTESIAN_POINT('Ctrl Pts',(-3.46632064065236,51.0874433129551,1.74319460026445));
#15134=CARTESIAN_POINT('Ctrl Pts',(-0.965959409052926,53.5021157627911,
1.58440988103877));
#15135=CARTESIAN_POINT('Ctrl Pts',(2.41872209844688,52.7106678650022,1.42562516181309));
#15136=CARTESIAN_POINT('Ctrl Pts',(3.58910270149602,49.4376309512673,1.2668404425874));
#15137=CARTESIAN_POINT('Ctrl Pts',(1.47372061005109,46.6794679460814,1.10805572336172));
#15138=CARTESIAN_POINT('Ctrl Pts',(-1.99083139973657,46.9611292918785,0.949271004136037));
#15139=CARTESIAN_POINT('Ctrl Pts',(-3.63280412987848,50.0249608192598,0.790486284910355));
#15140=CARTESIAN_POINT('Ctrl Pts',(-1.94901659367837,53.0656756689436,0.631701565684669));
#15141=CARTESIAN_POINT('Ctrl Pts',(1.51908697082356,53.300340014212,0.472916846458987));
#15142=CARTESIAN_POINT('Ctrl Pts',(3.59644503276003,50.5125594541255,0.314132127233302));
#15143=CARTESIAN_POINT('Ctrl Pts',(2.38140827918422,47.2575938852802,0.155347408007618));
#15144=CARTESIAN_POINT('Ctrl Pts',(-1.01394043867063,46.5091701825966,-0.00343731121806435));
#15145=CARTESIAN_POINT('Ctrl Pts',(-3.4807982360798,48.9648881946463,-0.162222030443749));
#15146=CARTESIAN_POINT('Ctrl Pts',(-3.00028114559473,51.2204253757917,-0.268078509927538));
#15147=CARTESIAN_POINT('Ctrl Pts',(-2.33606265769613,51.9973015569307,-0.321006749669432));
#15148=CARTESIAN_POINT('Ctrl Pts',(-0.745932854346969,47.2098224301579,
10.1070022498898));
#15149=CARTESIAN_POINT('Ctrl Pts',(-1.67382855441198,47.4578883222957,10.0540740101479));
#15150=CARTESIAN_POINT('Ctrl Pts',(-3.24653322010411,48.9488229706986,9.94821753066412));
#15151=CARTESIAN_POINT('Ctrl Pts',(-2.64331966248816,52.1636222989576,9.78943281143846));
#15152=CARTESIAN_POINT('Ctrl Pts',(0.384441012329826,53.3913294780743,9.63064809221275));
#15153=CARTESIAN_POINT('Ctrl Pts',(3.05794435580772,51.5174029217061,9.47186337298709));
#15154=CARTESIAN_POINT('Ctrl Pts',(2.93311447162684,48.2527764219532,9.31307865376139));
#15155=CARTESIAN_POINT('Ctrl Pts',(0.122478163952854,46.5884834525023,9.15429393453571));
#15156=CARTESIAN_POINT('Ctrl Pts',(-2.79998724422497,48.0469835444409,8.99550921531002));
#15157=CARTESIAN_POINT('Ctrl Pts',(-3.15926110240105,51.2936371775124,8.83672449608434));
#15158=CARTESIAN_POINT('Ctrl Pts',(-0.626207489574883,53.3558865860772,
8.67793977685865));
#15159=CARTESIAN_POINT('Ctrl Pts',(2.48009024000282,52.3459282171011,8.51915505763298));
#15160=CARTESIAN_POINT('Ctrl Pts',(3.31592579189812,49.1882855489611,8.36037033840729));
#15161=CARTESIAN_POINT('Ctrl Pts',(1.11607621235651,46.7737670839123,8.20158561918161));
#15162=CARTESIAN_POINT('Ctrl Pts',(-2.10551772393265,47.3128049682377,8.04280089995592));
#15163=CARTESIAN_POINT('Ctrl Pts',(-3.39954748337958,50.311928846849,7.88401618073025));
#15164=CARTESIAN_POINT('Ctrl Pts',(-1.5813464061563,53.0254853334235,7.72523146150455));
#15165=CARTESIAN_POINT('Ctrl Pts',(1.6845505393665,52.9692608282246,7.56644674227887));
#15166=CARTESIAN_POINT('Ctrl Pts',(3.40826961917741,50.1947266534715,7.40766202305319));
#15167=CARTESIAN_POINT('Ctrl Pts',(2.01177399977108,47.2419236622003,7.24887730382751));
#15168=CARTESIAN_POINT('Ctrl Pts',(-1.22646740026446,46.814093886757,7.09009258460182));
#15169=CARTESIAN_POINT('Ctrl Pts',(-3.34189819772363,49.3029085851684,6.93130786537614));
#15170=CARTESIAN_POINT('Ctrl Pts',(-2.39787637930257,52.4298989302782,6.77252314615045));
#15171=CARTESIAN_POINT('Ctrl Pts',(0.741361642631027,53.3323569589307,6.61373842692478));
#15172=CARTESIAN_POINT('Ctrl Pts',(3.20189533287493,51.1840972322951,6.45495370769908));
#15173=CARTESIAN_POINT('Ctrl Pts',(2.73114673582125,47.9518160534629,6.29616898847341));
#15174=CARTESIAN_POINT('Ctrl Pts',(-0.239921580162412,46.5946134415093,
6.13738426924771));
#15175=CARTESIAN_POINT('Ctrl Pts',(-2.99134565352125,48.3549859705726,5.97859955002204));
#15176=CARTESIAN_POINT('Ctrl Pts',(-3.00424219532036,51.6213416688123,5.81981483079635));
#15177=CARTESIAN_POINT('Ctrl Pts',(-0.266804635119595,53.4033858527374,
5.66103011157067));
#15178=CARTESIAN_POINT('Ctrl Pts',(2.71488816122889,52.0696865095247,5.50224539234499));
#15179=CARTESIAN_POINT('Ctrl Pts',(3.21114569366885,48.8412233564401,5.3434606731193));
#15180=CARTESIAN_POINT('Ctrl Pts',(0.767652389091321,46.6736010784556,5.18467595389362));
#15181=CARTESIAN_POINT('Ctrl Pts',(-2.37861399671836,47.5512420637604,5.02589123466794));
#15182=CARTESIAN_POINT('Ctrl Pts',(-3.34729856129375,50.6706804881919,4.86710651544225));
#15183=CARTESIAN_POINT('Ctrl Pts',(-1.25158658765491,53.1761220047933,4.70832179621657));
#15184=CARTESIAN_POINT('Ctrl Pts',(1.98993223179098,52.773876292935,4.54953707699088));
#15185=CARTESIAN_POINT('Ctrl Pts',(3.40970096509391,49.832192657113,4.3907523577652));
#15186=CARTESIAN_POINT('Ctrl Pts',(1.70794479033487,47.0441338715863,4.23196763853952));
#15187=CARTESIAN_POINT('Ctrl Pts',(-1.55740662611146,46.9621216982713,4.07318291931384));
#15188=CARTESIAN_POINT('Ctrl Pts',(-3.39697800345581,49.6612369266132,3.91439820008815));
#15189=CARTESIAN_POINT('Ctrl Pts',(-2.12667213392151,52.6704841531413,3.75561348086247));
#15190=CARTESIAN_POINT('Ctrl Pts',(1.09056694327298,53.234947250525,3.59682876163679));
#15191=CARTESIAN_POINT('Ctrl Pts',(3.3094099992828,50.837869581058,3.4380440424111));
#15192=CARTESIAN_POINT('Ctrl Pts',(2.49854286950392,47.6737361464895,3.27925932318542));
#15193=CARTESIAN_POINT('Ctrl Pts',(-0.599698983006457,46.6392588508537,
3.12047460395973));
#15194=CARTESIAN_POINT('Ctrl Pts',(-3.14892632391411,48.6814845426992,2.96168988473405));
#15195=CARTESIAN_POINT('Ctrl Pts',(-2.81536363139498,51.9307893902053,2.80290516550836));
#15196=CARTESIAN_POINT('Ctrl Pts',(0.095617955020209,53.4124883762385,2.64412044628269));
#15197=CARTESIAN_POINT('Ctrl Pts',(2.91906288933533,51.7701107633945,2.485335727057));
#15198=CARTESIAN_POINT('Ctrl Pts',(3.0701539567666,48.5072257144969,2.32655100783131));
#15199=CARTESIAN_POINT('Ctrl Pts',(0.410569817425986,46.610951404296,2.16776628860563));
#15200=CARTESIAN_POINT('Ctrl Pts',(-2.62488425534856,47.8172940318787,2.00898156937995));
#15201=CARTESIAN_POINT('Ctrl Pts',(-3.25730005866627,51.0218700271244,1.85019685015426));
#15202=CARTESIAN_POINT('Ctrl Pts',(-0.907711653352754,53.2909367199938,
1.69141213092858));
#15203=CARTESIAN_POINT('Ctrl Pts',(2.27287214597831,52.547213460909,1.5326274117029));
#15204=CARTESIAN_POINT('Ctrl Pts',(3.37267830997368,49.4715420397218,1.37384269247722));
#15205=CARTESIAN_POINT('Ctrl Pts',(1.38485464191613,46.8796974154137,1.21505797325153));
#15206=CARTESIAN_POINT('Ctrl Pts',(-1.87078343506508,47.1443744644522,1.05627325402585));
#15207=CARTESIAN_POINT('Ctrl Pts',(-3.41374452397723,50.0234556714361,0.897488534800164));
#15208=CARTESIAN_POINT('Ctrl Pts',(-1.83149007927186,52.88081414604,0.738703815574481));
#15209=CARTESIAN_POINT('Ctrl Pts',(1.4274853921914,53.1013281333051,0.579919096348797));
#15210=CARTESIAN_POINT('Ctrl Pts',(3.3795778955967,50.4816519050236,0.421134377123114));
#15211=CARTESIAN_POINT('Ctrl Pts',(2.23780836559748,47.4229621190836,0.262349657897429));
#15212=CARTESIAN_POINT('Ctrl Pts',(-0.952799406850132,46.7196686781745,
0.103564938671747));
#15213=CARTESIAN_POINT('Ctrl Pts',(-3.27090464904435,49.0273058687178,-0.0552197805539384));
#15214=CARTESIAN_POINT('Ctrl Pts',(-2.81936293975441,51.1468332160454,-0.161076260037727));
#15215=CARTESIAN_POINT('Ctrl Pts',(-2.1951971040191,51.8768634390788,-0.214004499779622));
#15216=CARTESIAN_POINT('Ctrl Pts',(-0.698066426161048,47.3888678140614,
10.2140044997796));
#15217=CARTESIAN_POINT('Ctrl Pts',(-1.56641916249635,47.6210153455288,10.1610762600377));
#15218=CARTESIAN_POINT('Ctrl Pts',(-3.03820354494941,49.016276883595,10.0552197805539));
#15219=CARTESIAN_POINT('Ctrl Pts',(-2.47369813414337,52.0247828970048,9.89643506132825));
#15220=CARTESIAN_POINT('Ctrl Pts',(0.359771475385354,53.1737082431722,9.73765034210257));
#15221=CARTESIAN_POINT('Ctrl Pts',(2.86171640707103,51.4200313452195,9.57886562287689));
#15222=CARTESIAN_POINT('Ctrl Pts',(2.74489684265523,48.3648955643612,9.4200809036512));
#15223=CARTESIAN_POINT('Ctrl Pts',(0.114618753812882,46.807400089401,9.26129618442552));
#15224=CARTESIAN_POINT('Ctrl Pts',(-2.62031237460883,48.1723083928789,9.10251146519984));
#15225=CARTESIAN_POINT('Ctrl Pts',(-2.95653166931952,51.210624623909,8.94372674597415));
#15226=CARTESIAN_POINT('Ctrl Pts',(-0.586023824712095,53.1405397176071,
8.78494202674847));
#15227=CARTESIAN_POINT('Ctrl Pts',(2.32094312551941,52.1953902646851,8.62615730752278));
#15228=CARTESIAN_POINT('Ctrl Pts',(3.10314320313993,49.2403731748803,8.46737258829711));
#15229=CARTESIAN_POINT('Ctrl Pts',(1.04445772611147,46.9807940908192,8.30858786907141));
#15230=CARTESIAN_POINT('Ctrl Pts',(-1.97040688608782,47.4852419741422,8.14980314984574));
#15231=CARTESIAN_POINT('Ctrl Pts',(-3.1813988999923,50.2919124074875,7.99101843062005));
#15232=CARTESIAN_POINT('Ctrl Pts',(-1.47987158339412,52.8313402765381,7.83223371139436));
#15233=CARTESIAN_POINT('Ctrl Pts',(1.57645311887049,52.7787236915758,7.67344899216869));
#15234=CARTESIAN_POINT('Ctrl Pts',(3.1895613373074,50.1822310658057,7.514664272943));
#15235=CARTESIAN_POINT('Ctrl Pts',(1.88267868626508,47.418909113619,7.35587955371732));
#15236=CARTESIAN_POINT('Ctrl Pts',(-1.14776512378607,47.0185331272166,7.19709483449163));
#15237=CARTESIAN_POINT('Ctrl Pts',(-3.12744896257627,49.3476408636202,7.03831011526595));
#15238=CARTESIAN_POINT('Ctrl Pts',(-2.2440049191038,52.2739725865498,6.87952539604026));
#15239=CARTESIAN_POINT('Ctrl Pts',(0.693788548591803,53.118519984014,6.72074067681459));
#15240=CARTESIAN_POINT('Ctrl Pts',(2.99643006597223,51.1081138447764,6.5619559575889));
#15241=CARTESIAN_POINT('Ctrl Pts',(2.55588935396233,48.0832477891978,6.40317123836322));
#15242=CARTESIAN_POINT('Ctrl Pts',(-0.224525839084415,46.8131367176962,
6.24438651913753));
#15243=CARTESIAN_POINT('Ctrl Pts',(-2.79939133609292,48.4605463376293,6.08560179991184));
#15244=CARTESIAN_POINT('Ctrl Pts',(-2.81146030824111,51.5173003544999,5.92681708068617));
#15245=CARTESIAN_POINT('Ctrl Pts',(-0.249683811399071,53.184990961616,5.76803236146048));
#15246=CARTESIAN_POINT('Ctrl Pts',(2.54067409029078,51.9368749567177,5.6092476422348));
#15247=CARTESIAN_POINT('Ctrl Pts',(3.00508683214425,48.9155819245998,5.45046292300911));
#15248=CARTESIAN_POINT('Ctrl Pts',(0.718392220779847,46.8870557267768,5.29167820378344));
#15249=CARTESIAN_POINT('Ctrl Pts',(-2.2259786014647,47.708378587801,5.13289348455774));
#15250=CARTESIAN_POINT('Ctrl Pts',(-3.13250278541755,50.627642995961,4.97410876533206));
#15251=CARTESIAN_POINT('Ctrl Pts',(-1.1712724157193,52.9723106094831,4.81532404610638));
#15252=CARTESIAN_POINT('Ctrl Pts',(1.86223850210367,52.5958769601551,4.65653932688069));
#15253=CARTESIAN_POINT('Ctrl Pts',(3.19090083391586,49.8429608356167,4.49775460765502));
#15254=CARTESIAN_POINT('Ctrl Pts',(1.59834616335972,47.23381147184,4.33896988842933));
#15255=CARTESIAN_POINT('Ctrl Pts',(-1.45746801636849,47.1570620105525,4.18018516920365));
#15256=CARTESIAN_POINT('Ctrl Pts',(-3.17899430330907,49.6829753153031,4.02140044997796));
#15257=CARTESIAN_POINT('Ctrl Pts',(-1.99020381994374,52.4991194824566,3.86261573075228));
#15258=CARTESIAN_POINT('Ctrl Pts',(1.02058538398395,53.0273610457479,3.70383101152659));
#15259=CARTESIAN_POINT('Ctrl Pts',(3.09704552821105,50.7841035833584,3.54504629230091));
#15260=CARTESIAN_POINT('Ctrl Pts',(2.33821165184056,47.8230122388839,3.38626157307523));
#15261=CARTESIAN_POINT('Ctrl Pts',(-0.561216366057806,46.8549172360953,
3.22747685384954));
#15262=CARTESIAN_POINT('Ctrl Pts',(-2.94686007241706,48.7660935327458,3.06869213462386));
#15263=CARTESIAN_POINT('Ctrl Pts',(-2.63470206072667,51.8068908500756,2.90990741539818));
#15264=CARTESIAN_POINT('Ctrl Pts',(0.0894821614959184,53.1935093771978,
2.75112269617249));
#15265=CARTESIAN_POINT('Ctrl Pts',(2.73174694883439,51.6565229528518,2.59233797694681));
#15266=CARTESIAN_POINT('Ctrl Pts',(2.87314251929621,48.6030168741415,2.43355325772113));
#15267=CARTESIAN_POINT('Ctrl Pts',(0.384223597968559,46.8284262752304,2.27476853849544));
#15268=CARTESIAN_POINT('Ctrl Pts',(-2.4564457250267,47.9573580307564,2.11598381926976));
#15269=CARTESIAN_POINT('Ctrl Pts',(-3.04827947668019,50.9562967412935,1.95719910004407));
#15270=CARTESIAN_POINT('Ctrl Pts',(-0.849463897652582,53.0797576771966,
1.79841438081839));
#15271=CARTESIAN_POINT('Ctrl Pts',(2.12702219350974,52.3837590568159,1.63962966159271));
#15272=CARTESIAN_POINT('Ctrl Pts',(3.15625391845133,49.5054531281764,1.48084494236703));
#15273=CARTESIAN_POINT('Ctrl Pts',(1.29598867378117,47.0799268847461,1.32206022314134));
#15274=CARTESIAN_POINT('Ctrl Pts',(-1.75073547039358,47.3276196370259,1.16327550391566));
#15275=CARTESIAN_POINT('Ctrl Pts',(-3.19468491807599,50.0219505236124,1.00449078468998));
#15276=CARTESIAN_POINT('Ctrl Pts',(-1.71396356486536,52.6959526231364,0.84570606546429));
#15277=CARTESIAN_POINT('Ctrl Pts',(1.33588381355923,52.9023162523982,0.686921346238609));
#15278=CARTESIAN_POINT('Ctrl Pts',(3.16271075843336,50.4507443559217,0.528136627012924));
#15279=CARTESIAN_POINT('Ctrl Pts',(2.09420845201075,47.588330352887,0.36935190778724));
#15280=CARTESIAN_POINT('Ctrl Pts',(-0.891658375029637,46.9301671737524,
0.210567188561557));
#15281=CARTESIAN_POINT('Ctrl Pts',(-3.0610110620089,49.0897235427894,0.0517824693358723));
#15282=CARTESIAN_POINT('Ctrl Pts',(-2.63844473391409,51.0732410562992,-0.0540740101479162));
#15283=CARTESIAN_POINT('Ctrl Pts',(-2.05433155034207,51.7564253212269,-0.107002249889811));
#15284=CARTESIAN_POINT('Ctrl Pts',(-0.650199997975127,47.5679131979649,
10.3210067496694));
#15285=CARTESIAN_POINT('Ctrl Pts',(-1.4590097705807,47.784142368762,10.2680785099275));
#15286=CARTESIAN_POINT('Ctrl Pts',(-2.82987386979471,49.0837307964915,10.1622220304437));
#15287=CARTESIAN_POINT('Ctrl Pts',(-2.30407660579858,51.8859434950519,10.0034373112181));
#15288=CARTESIAN_POINT('Ctrl Pts',(0.335101938440882,52.95608700827,9.84465259199238));
#15289=CARTESIAN_POINT('Ctrl Pts',(2.66548845833433,51.3226597687329,9.68586787276669));
#15290=CARTESIAN_POINT('Ctrl Pts',(2.55667921368362,48.4770147067691,9.52708315354102));
#15291=CARTESIAN_POINT('Ctrl Pts',(0.106759343672908,47.0263167262997,9.36829843431533));
#15292=CARTESIAN_POINT('Ctrl Pts',(-2.44063750499268,48.2976332413169,9.20951371508965));
#15293=CARTESIAN_POINT('Ctrl Pts',(-2.75380223623798,51.1276120703055,9.05072899586396));
#15294=CARTESIAN_POINT('Ctrl Pts',(-0.545840159849303,52.9251928491371,
8.89194427663828));
#15295=CARTESIAN_POINT('Ctrl Pts',(2.16179601103599,52.0448523122691,8.73315955741259));
#15296=CARTESIAN_POINT('Ctrl Pts',(2.89036061438174,49.2924608007996,8.57437483818692));
#15297=CARTESIAN_POINT('Ctrl Pts',(0.972839239866417,47.187821097726,8.41559011896123));
#15298=CARTESIAN_POINT('Ctrl Pts',(-1.83529604824299,47.6576789800468,8.25680539973555));
#15299=CARTESIAN_POINT('Ctrl Pts',(-2.96325031660503,50.2718959681259,8.09802068050987));
#15300=CARTESIAN_POINT('Ctrl Pts',(-1.37839676063194,52.6371952196527,7.93923596128418));
#15301=CARTESIAN_POINT('Ctrl Pts',(1.46835569837446,52.5881865549271,7.78045124205849));
#15302=CARTESIAN_POINT('Ctrl Pts',(2.9708530554374,50.1697354781399,7.62166652283282));
#15303=CARTESIAN_POINT('Ctrl Pts',(1.75358337275908,47.5958945650376,7.46288180360712));
#15304=CARTESIAN_POINT('Ctrl Pts',(-1.06906284730768,47.2229723676763,7.30409708438145));
#15305=CARTESIAN_POINT('Ctrl Pts',(-2.9129997274289,49.3923731420721,7.14531236515576));
#15306=CARTESIAN_POINT('Ctrl Pts',(-2.09013345890504,52.1180462428214,6.98652764593008));
#15307=CARTESIAN_POINT('Ctrl Pts',(0.646215454552581,52.9046830090973,6.82774292670439));
#15308=CARTESIAN_POINT('Ctrl Pts',(2.79096479906952,51.0321304572577,6.66895820747871));
#15309=CARTESIAN_POINT('Ctrl Pts',(2.38063197210341,48.2146795249326,6.51017348825303));
#15310=CARTESIAN_POINT('Ctrl Pts',(-0.20913009800642,47.031659993883,6.35138876902734));
#15311=CARTESIAN_POINT('Ctrl Pts',(-2.60743701866458,48.5661067046858,6.19260404980165));
#15312=CARTESIAN_POINT('Ctrl Pts',(-2.61867842116187,51.4132590401875,6.03381933057598));
#15313=CARTESIAN_POINT('Ctrl Pts',(-0.232562987678543,52.9665960704945,
5.87503461135029));
#15314=CARTESIAN_POINT('Ctrl Pts',(2.36646001935266,51.8040634039108,5.71624989212461));
#15315=CARTESIAN_POINT('Ctrl Pts',(2.79902797061965,48.9899404927595,5.55746517289893));
#15316=CARTESIAN_POINT('Ctrl Pts',(0.66913205246837,47.1005103750979,5.39868045367324));
#15317=CARTESIAN_POINT('Ctrl Pts',(-2.07334320621103,47.8655151118416,5.23989573444756));
#15318=CARTESIAN_POINT('Ctrl Pts',(-2.91770700954136,50.5846055037301,5.08111101522187));
#15319=CARTESIAN_POINT('Ctrl Pts',(-1.09095824378368,52.7684992141729,4.92232629599619));
#15320=CARTESIAN_POINT('Ctrl Pts',(1.73454477241634,52.4178776273751,4.7635415767705));
#15321=CARTESIAN_POINT('Ctrl Pts',(2.97210070273781,49.8537290141204,4.60475685754483));
#15322=CARTESIAN_POINT('Ctrl Pts',(1.48874753638457,47.4234890720937,4.44597213831914));
#15323=CARTESIAN_POINT('Ctrl Pts',(-1.35752940662552,47.3520023228338,4.28718741909346));
#15324=CARTESIAN_POINT('Ctrl Pts',(-2.96101060316233,49.7047137039929,4.12840269986777));
#15325=CARTESIAN_POINT('Ctrl Pts',(-1.85373550596597,52.327754811772,3.96961798064209));
#15326=CARTESIAN_POINT('Ctrl Pts',(0.950603824694923,52.8197748409707,3.8108332614164));
#15327=CARTESIAN_POINT('Ctrl Pts',(2.88468105713929,50.7303375856587,3.65204854219073));
#15328=CARTESIAN_POINT('Ctrl Pts',(2.1778804341772,47.9722883312785,3.49326382296504));
#15329=CARTESIAN_POINT('Ctrl Pts',(-0.522733749109153,47.0705756213368,
3.33447910373936));
#15330=CARTESIAN_POINT('Ctrl Pts',(-2.74479382092,48.8507025227925,3.17569438451367));
#15331=CARTESIAN_POINT('Ctrl Pts',(-2.45404049005835,51.6829923099458,3.01690966528799));
#15332=CARTESIAN_POINT('Ctrl Pts',(0.0833463679716227,52.974530378157,2.85812494606231));
#15333=CARTESIAN_POINT('Ctrl Pts',(2.54443100833344,51.5429351423091,2.69934022683662));
#15334=CARTESIAN_POINT('Ctrl Pts',(2.67613108182581,48.6988080337859,2.54055550761094));
#15335=CARTESIAN_POINT('Ctrl Pts',(0.357877378511138,47.0459011461649,2.38177078838525));
#15336=CARTESIAN_POINT('Ctrl Pts',(-2.28800719470483,48.0974220296341,2.22298606915957));
#15337=CARTESIAN_POINT('Ctrl Pts',(-2.8392588946941,50.8907234554627,2.06420134993389));
#15338=CARTESIAN_POINT('Ctrl Pts',(-0.791216141952413,52.8685786343994,
1.9054166307082));
#15339=CARTESIAN_POINT('Ctrl Pts',(1.98117224104117,52.2203046527227,1.74663191148252));
#15340=CARTESIAN_POINT('Ctrl Pts',(2.93982952692898,49.539364216631,1.58784719225684));
#15341=CARTESIAN_POINT('Ctrl Pts',(1.20712270564621,47.2801563540783,1.42906247303115));
#15342=CARTESIAN_POINT('Ctrl Pts',(-1.63068750572208,47.5108648095996,1.27027775380547));
#15343=CARTESIAN_POINT('Ctrl Pts',(-2.97562531217475,50.0204453757886,1.11149303457979));
#15344=CARTESIAN_POINT('Ctrl Pts',(-1.59643705045885,52.5110911002329,0.952708315354101));
#15345=CARTESIAN_POINT('Ctrl Pts',(1.24428223492706,52.7033043714913,0.79392359612842));
#15346=CARTESIAN_POINT('Ctrl Pts',(2.94584362127002,50.4198368068199,0.635138876902735));
#15347=CARTESIAN_POINT('Ctrl Pts',(1.95060853842403,47.7536985866904,0.476354157677051));
#15348=CARTESIAN_POINT('Ctrl Pts',(-0.830517343209144,47.1406656693304,
0.317569438451368));
#15349=CARTESIAN_POINT('Ctrl Pts',(-2.85111747497345,49.1521412168609,0.158784719225683));
#15350=CARTESIAN_POINT('Ctrl Pts',(-2.45752652807377,50.999648896553,0.0529282397418946));
#15351=CARTESIAN_POINT('Ctrl Pts',(-1.91346599666504,51.635987203375,0.));
#15352=CARTESIAN_POINT('Ctrl Pts',(-1.91346599666504,51.635987203375,0.));
#15353=CARTESIAN_POINT('Ctrl Pts',(-1.97508250372926,51.5780828168137,-7.88547235160471E-17));
#15354=CARTESIAN_POINT('Ctrl Pts',(-2.03332802563557,51.517028168085,-1.95903716127754E-15));
#15355=CARTESIAN_POINT('Ctrl Pts',(-2.0882055508515,51.4532079963186,-1.60982338570648E-15));
#15356=CARTESIAN_POINT('Ctrl Pts',(-2.14453544714772,51.3876987802404,-1.25136742972581E-15));
#15357=CARTESIAN_POINT('Ctrl Pts',(-2.1973171511753,51.3192752892963,-2.54643214235558E-15));
#15358=CARTESIAN_POINT('Ctrl Pts',(-2.24652834894968,51.2483050710386,-2.88657986402541E-15));
#15359=CARTESIAN_POINT('Ctrl Pts',(-2.29743052792617,51.1748961942964,-3.23841564510647E-15));
#15360=CARTESIAN_POINT('Ctrl Pts',(-2.34451318991709,51.0987620412396,1.26930694503224E-15));
#15361=CARTESIAN_POINT('Ctrl Pts',(-2.38771671870761,51.0202653810526,9.99200722162641E-16));
#15362=CARTESIAN_POINT('Ctrl Pts',(-2.40661826255346,50.9859230922208,8.81029249657191E-16));
#15363=CARTESIAN_POINT('Ctrl Pts',(-2.42477682213031,50.9511280985978,-4.72647997039093E-15));
#15364=CARTESIAN_POINT('Ctrl Pts',(-2.44218496027157,50.9159086901715,-5.16253706450698E-15));
#15365=CARTESIAN_POINT('Ctrl Pts',(-2.4516917365468,50.8966749827102,-5.40067265392762E-15));
#15366=CARTESIAN_POINT('Ctrl Pts',(-2.4609746819567,50.8773146792715,1.38692847400875E-15));
#15367=CARTESIAN_POINT('Ctrl Pts',(-2.47003238168185,50.857832258915,1.60982338570648E-15));
#15368=CARTESIAN_POINT('Ctrl Pts',(-2.47868101112295,50.8392297174981,1.82265175870151E-15));
#15369=CARTESIAN_POINT('Ctrl Pts',(-2.48712676984399,50.8205098452481,-2.92077872961859E-16));
#15370=CARTESIAN_POINT('Ctrl Pts',(-2.49535433119684,50.801709305486,-2.22044604925031E-16));
#15371=CARTESIAN_POINT('Ctrl Pts',(-2.53191983250978,50.7181546369918,8.92021235434719E-17));
#15372=CARTESIAN_POINT('Ctrl Pts',(-2.56422492917263,50.6329165377822,5.94993583842564E-16));
#15373=CARTESIAN_POINT('Ctrl Pts',(-2.59224521232009,50.546393762837,5.82867087928207E-16));
#15374=CARTESIAN_POINT('Ctrl Pts',(-2.62072727043851,50.4584450903848,5.70540747056209E-16));
#15375=CARTESIAN_POINT('Ctrl Pts',(-2.64478261577045,50.3691682946478,1.3966825979773E-15));
#15376=CARTESIAN_POINT('Ctrl Pts',(-2.66434650648327,50.2789450457094,9.43689570931383E-16));
#15377=CARTESIAN_POINT('Ctrl Pts',(-2.68357149093349,50.1902847386492,4.98543764872047E-16));
#15378=CARTESIAN_POINT('Ctrl Pts',(-2.6984595431006,50.1007095761311,-1.44477158663301E-15));
#15379=CARTESIAN_POINT('Ctrl Pts',(-2.70890652948763,50.0105588921822,-1.74860126378462E-15));
#15380=CARTESIAN_POINT('Ctrl Pts',(-2.71303741983049,49.9749120007313,-1.86873993657737E-15));
#15381=CARTESIAN_POINT('Ctrl Pts',(-2.71647344141028,49.9391749440761,-4.57020580419667E-16));
#15382=CARTESIAN_POINT('Ctrl Pts',(-2.71920612755143,49.9033681666514,-7.21644966006352E-16));
#15383=CARTESIAN_POINT('Ctrl Pts',(-2.72082363900511,49.8821736826851,-8.78279483290925E-16));
#15384=CARTESIAN_POINT('Ctrl Pts',(-2.7221947068849,49.8609547672148,-1.34276899995115E-15));
#15385=CARTESIAN_POINT('Ctrl Pts',(-2.72331737293965,49.8397156372056,-1.41553435639707E-15));
#15386=CARTESIAN_POINT('Ctrl Pts',(-2.72406463156244,49.8255786434197,-1.46396776169497E-15));
#15387=CARTESIAN_POINT('Ctrl Pts',(-2.7247017593876,49.8114326986645,-2.92576848619345E-16));
#15388=CARTESIAN_POINT('Ctrl Pts',(-2.72522782764266,49.797293600135,-4.16333634234434E-16));
#15389=CARTESIAN_POINT('Ctrl Pts',(-2.72876903784861,49.7021167489681,-1.24939814261499E-15));
#15390=CARTESIAN_POINT('Ctrl Pts',(-2.72729103062767,49.6070885424556,8.33615584934857E-16));
#15391=CARTESIAN_POINT('Ctrl Pts',(-2.72073501618782,49.5126075692422,6.93889390390723E-16));
#15392=CARTESIAN_POINT('Ctrl Pts',(-2.71420165583577,49.4184530718599,5.54646015021133E-16));
#15393=CARTESIAN_POINT('Ctrl Pts',(-2.70262568072403,49.3248410792282,-1.79204710018197E-16));
#15394=CARTESIAN_POINT('Ctrl Pts',(-2.68590091265149,49.2321481599992,2.77555756156289E-16));
#15395=CARTESIAN_POINT('Ctrl Pts',(-2.68396405390562,49.2214135961171,3.30452184964298E-16));
#15396=CARTESIAN_POINT('Ctrl Pts',(-2.68195808574165,49.2106913478966,-6.33066629083406E-15));
#15397=CARTESIAN_POINT('Ctrl Pts',(-2.67988279801038,49.1999819937366,-6.41153796721028E-15));
#15398=CARTESIAN_POINT('Ctrl Pts',(-2.66233852493469,49.1094461942822,-7.09521895903373E-15));
#15399=CARTESIAN_POINT('Ctrl Pts',(-2.63984447556841,49.0198316064943,-8.66493849292325E-16));
#15400=CARTESIAN_POINT('Ctrl Pts',(-2.61267603168784,48.9313762482598,-1.11022302462516E-15));
#15401=CARTESIAN_POINT('Ctrl Pts',(-2.60192825571706,48.8963835052856,-1.20664174428155E-15));
#15402=CARTESIAN_POINT('Ctrl Pts',(-2.59044836827368,48.861572229629,-5.47531613863234E-16));
#15403=CARTESIAN_POINT('Ctrl Pts',(-2.57825122455276,48.8269574989795,-3.60822483003176E-16));
#15404=CARTESIAN_POINT('Ctrl Pts',(-2.57231287966207,48.8101048477688,-2.69920609691125E-16));
#15405=CARTESIAN_POINT('Ctrl Pts',(-2.56620450114377,48.7932987890619,-9.87740507932057E-16));
#15406=CARTESIAN_POINT('Ctrl Pts',(-2.55992770321574,48.7765410907625,-9.15933995315754E-16));
#15407=CARTESIAN_POINT('Ctrl Pts',(-2.55466778336413,48.762498237868,-8.55760558873183E-16));
#15408=CARTESIAN_POINT('Ctrl Pts',(-2.54929245582117,48.7484970704423,-1.04336745179747E-15));
#15409=CARTESIAN_POINT('Ctrl Pts',(-2.54380502947758,48.7345433945498,-9.43689570931383E-16));
#15410=CARTESIAN_POINT('Ctrl Pts',(-2.50958084575905,48.6475165922947,-3.22014874300647E-16));
#15411=CARTESIAN_POINT('Ctrl Pts',(-2.47097808219571,48.5622772719038,-2.76096825153635E-15));
#15412=CARTESIAN_POINT('Ctrl Pts',(-2.42832930579416,48.4790573924985,-2.45636844198316E-15));
#15413=CARTESIAN_POINT('Ctrl Pts',(-2.38409930402159,48.3927520931635,-2.14047543746612E-15));
#15414=CARTESIAN_POINT('Ctrl Pts',(-2.3355175823713,48.3086180283362,-4.37014208287737E-16));
#15415=CARTESIAN_POINT('Ctrl Pts',(-2.28289912148411,48.2269174441202,-1.9151347174784E-15));
#15416=CARTESIAN_POINT('Ctrl Pts',(-2.2297022750075,48.1443188016988,-3.40950282470803E-15));
#15417=CARTESIAN_POINT('Ctrl Pts',(-2.17237903905252,48.0642066138853,1.84196985151739E-15));
#15418=CARTESIAN_POINT('Ctrl Pts',(-2.11120327391795,47.9868672202785,1.81799020282369E-15));
#15419=CARTESIAN_POINT('Ctrl Pts',(-2.08739408923495,47.9567672631859,1.80865748940155E-15));
#15420=CARTESIAN_POINT('Ctrl Pts',(-2.06300084281701,47.9270875343801,-2.70289509530768E-15));
#15421=CARTESIAN_POINT('Ctrl Pts',(-2.03803781529234,47.8978459523877,-2.88657986402541E-15));
#15422=CARTESIAN_POINT('Ctrl Pts',(-2.01823971473763,47.8746545434093,-3.03225969063487E-15));
#15423=CARTESIAN_POINT('Ctrl Pts',(-1.99808319977527,47.8517387409254,-3.30551557830788E-15));
#15424=CARTESIAN_POINT('Ctrl Pts',(-1.97757497212805,47.8291078145036,-3.4555691641458E-15));
#15425=CARTESIAN_POINT('Ctrl Pts',(-1.96583741766514,47.8161553675154,-3.54144992217255E-15));
#15426=CARTESIAN_POINT('Ctrl Pts',(-1.95398941490868,47.8033015714534,1.65071552113353E-15));
#15427=CARTESIAN_POINT('Ctrl Pts',(-1.9420381151495,47.7905538223288,1.48492329543615E-15));
#15428=CARTESIAN_POINT('Ctrl Pts',(-1.87298185596159,47.7168955688038,5.26952937416942E-16));
#15429=CARTESIAN_POINT('Ctrl Pts',(-1.80042495380938,47.6467145489693,-8.25147557761074E-16));
#15430=CARTESIAN_POINT('Ctrl Pts',(-1.72467948086462,47.5802997238268,-1.94289029309402E-16));
#15431=CARTESIAN_POINT('Ctrl Pts',(-1.66042054073069,47.5239564717893,3.4090203672718E-16));
#15432=CARTESIAN_POINT('Ctrl Pts',(-1.59386571260425,47.4703237412601,1.07379577703767E-16));
#15433=CARTESIAN_POINT('Ctrl Pts',(-1.52518066669226,47.4195928883885,-7.35522753814166E-16));
#15434=CARTESIAN_POINT('Ctrl Pts',(-1.50256447612399,47.4028885443642,-1.01306846273714E-15));
#15435=CARTESIAN_POINT('Ctrl Pts',(-1.47971715840407,47.3864989618495,-1.85072163263063E-15));
#15436=CARTESIAN_POINT('Ctrl Pts',(-1.45664416191384,47.3704314082844,-2.14411821630733E-15));
#15437=CARTESIAN_POINT('Ctrl Pts',(-1.43995378600627,47.3588085785826,-2.35635329698423E-15));
#15438=CARTESIAN_POINT('Ctrl Pts',(-1.42314427660525,47.347353683751,-3.1683259339951E-15));
#15439=CARTESIAN_POINT('Ctrl Pts',(-1.4062324772292,47.3360791105664,-3.08086889333481E-15));
#15440=CARTESIAN_POINT('Ctrl Pts',(-1.31987495994381,47.278507226758,-2.634282889527E-15));
#15441=CARTESIAN_POINT('Ctrl Pts',(-1.23076834239895,47.2255739050535,4.26208680824903E-15));
#15442=CARTESIAN_POINT('Ctrl Pts',(-1.13922130482109,47.1776007437286,2.75127143289922E-15));
#15443=CARTESIAN_POINT('Ctrl Pts',(-1.04767426724323,47.1296275824037,1.2404560575494E-15));
#15444=CARTESIAN_POINT('Ctrl Pts',(-0.953686164033146,47.0866136704993,
-2.39983802697838E-15));
#15445=CARTESIAN_POINT('Ctrl Pts',(-0.857527633333973,47.0489213548329,
-3.9118014383277E-15));
#15446=CARTESIAN_POINT('Ctrl Pts',(-0.836959291797765,47.0408589560391,
-4.28706450102705E-15));
#15447=CARTESIAN_POINT('Ctrl Pts',(-0.816291527885438,47.0330402152543,
-8.74346376558217E-17));
#15448=CARTESIAN_POINT('Ctrl Pts',(-0.795528245027205,47.0254639548254,
-5.55111512312578E-17));
#15449=CARTESIAN_POINT('Ctrl Pts',(-2.51421069693398,50.0014124180709,9.11258330249199));
#15450=CARTESIAN_POINT('Ctrl Pts',(-2.51589016857918,50.3285491477533,9.09196520028265));
#15451=CARTESIAN_POINT('Ctrl Pts',(-2.45663359423571,50.6551027847351,9.07134709807331));
#15452=CARTESIAN_POINT('Ctrl Pts',(-2.33361443496565,50.9555457286126,9.05072899586397));
#15453=CARTESIAN_POINT('Ctrl Pts',(-2.01781487744175,51.7268056632493,8.99780075612207));
#15454=CARTESIAN_POINT('Ctrl Pts',(-1.28182751864553,52.3259992561932,8.94487251638018));
#15455=CARTESIAN_POINT('Ctrl Pts',(-0.462561144099867,52.4788726298538,
8.89194427663828));
#15456=CARTESIAN_POINT('Ctrl Pts',(0.356705230445793,52.6317460035144,8.83901603689639));
#15457=CARTESIAN_POINT('Ctrl Pts',(1.25925062074089,52.3382991578918,8.78608779715449));
#15458=CARTESIAN_POINT('Ctrl Pts',(1.83195074977939,51.7328438165022,8.7331595574126));
#15459=CARTESIAN_POINT('Ctrl Pts',(2.4046508788179,51.1273884751126,8.6802313176707));
#15460=CARTESIAN_POINT('Ctrl Pts',(2.64750574659982,50.2099246379561,8.62730307792881));
#15461=CARTESIAN_POINT('Ctrl Pts',(2.44934628473822,49.4004194355323,8.57437483818692));
#15462=CARTESIAN_POINT('Ctrl Pts',(2.25118682287662,48.5909142331084,8.52144659844502));
#15463=CARTESIAN_POINT('Ctrl Pts',(1.61201303137152,47.8893676654172,8.46851835870313));
#15464=CARTESIAN_POINT('Ctrl Pts',(0.824403587600737,47.6169040286251,8.41559011896123));
#15465=CARTESIAN_POINT('Ctrl Pts',(0.0367941438299503,47.3444403918329,
8.36266187921934));
#15466=CARTESIAN_POINT('Ctrl Pts',(-0.899250952206518,47.5010596859399,
8.30973363947744));
#15467=CARTESIAN_POINT('Ctrl Pts',(-1.55526587828509,48.0150721643398,8.25680539973555));
#15468=CARTESIAN_POINT('Ctrl Pts',(-2.15111571146493,48.4819430194556,8.20873136732103));
#15469=CARTESIAN_POINT('Ctrl Pts',(-2.51594477493577,49.2436579927481,8.16065733490651));
#15470=CARTESIAN_POINT('Ctrl Pts',(-2.52079116141582,50.0013273547755,8.11258330249199));
#15471=CARTESIAN_POINT('Ctrl Pts',(-0.79379928253289,47.0307770462543,10.));
#15472=CARTESIAN_POINT('Ctrl Pts',(-0.88685746467595,47.0648181449704,10.));
#15473=CARTESIAN_POINT('Ctrl Pts',(-0.977848397661759,47.1036281235935,
10.));
#15474=CARTESIAN_POINT('Ctrl Pts',(-1.06656423869436,47.1468784092156,10.));
#15475=CARTESIAN_POINT('Ctrl Pts',(-1.15724789156607,47.1910880322357,10.));
#15476=CARTESIAN_POINT('Ctrl Pts',(-1.24555507223239,47.2399377454417,10.));
#15477=CARTESIAN_POINT('Ctrl Pts',(-1.33123485996843,47.2931221720949,10.));
#15478=CARTESIAN_POINT('Ctrl Pts',(-1.41418373231515,47.3446114245062,10.));
#15479=CARTESIAN_POINT('Ctrl Pts',(-1.49467035617305,47.4001643315653,10.));
#15480=CARTESIAN_POINT('Ctrl Pts',(-1.57243333752743,47.4595344816828,10.));
#15481=CARTESIAN_POINT('Ctrl Pts',(-1.64047594621252,47.5114833630356,10.));
#15482=CARTESIAN_POINT('Ctrl Pts',(-1.70643296936772,47.5663555378622,10.));
#15483=CARTESIAN_POINT('Ctrl Pts',(-1.77010402938273,47.6239989062131,10.));
#15484=CARTESIAN_POINT('Ctrl Pts',(-1.78344377116941,47.6360757846149,10.));
#15485=CARTESIAN_POINT('Ctrl Pts',(-1.79668493788908,47.648276201783,10.));
#15486=CARTESIAN_POINT('Ctrl Pts',(-1.80980851672957,47.6605824648445,10.));
#15487=CARTESIAN_POINT('Ctrl Pts',(-1.88223677518892,47.7285000056708,10.));
#15488=CARTESIAN_POINT('Ctrl Pts',(-1.95119933213202,47.7997385749445,10.));
#15489=CARTESIAN_POINT('Ctrl Pts',(-2.01645680990078,47.8740071988597,10.));
#15490=CARTESIAN_POINT('Ctrl Pts',(-2.08135213335938,47.9478636600132,10.));
#15491=CARTESIAN_POINT('Ctrl Pts',(-2.14258387218845,48.0247174355525,10.));
#15492=CARTESIAN_POINT('Ctrl Pts',(-2.19987299961007,48.1043091145767,10.));
#15493=CARTESIAN_POINT('Ctrl Pts',(-2.25572878425838,48.1819094531306,10.));
#15494=CARTESIAN_POINT('Ctrl Pts',(-2.30783704358244,48.2621131469488,10.));
#15495=CARTESIAN_POINT('Ctrl Pts',(-2.35589231127005,48.3446938995333,10.));
#15496=CARTESIAN_POINT('Ctrl Pts',(-2.37661982896018,48.3803131790093,10.));
#15497=CARTESIAN_POINT('Ctrl Pts',(-2.39659269249857,48.4163748099892,10.));
#15498=CARTESIAN_POINT('Ctrl Pts',(-2.41578340672494,48.4528609664052,10.));
#15499=CARTESIAN_POINT('Ctrl Pts',(-2.42944475906872,48.4788344779999,10.));
#15500=CARTESIAN_POINT('Ctrl Pts',(-2.44270970882733,48.5050231267819,10.));
#15501=CARTESIAN_POINT('Ctrl Pts',(-2.45556774116037,48.531420485817,10.));
#15502=CARTESIAN_POINT('Ctrl Pts',(-2.46118157523555,48.542945607998,10.));
#15503=CARTESIAN_POINT('Ctrl Pts',(-2.46671692321559,48.5545087352933,10.));
#15504=CARTESIAN_POINT('Ctrl Pts',(-2.47216920778115,48.5661010414056,10.));
#15505=CARTESIAN_POINT('Ctrl Pts',(-2.51239820905703,48.65163342545,10.));
#15506=CARTESIAN_POINT('Ctrl Pts',(-2.54817121352112,48.7388794985857,10.));
#15507=CARTESIAN_POINT('Ctrl Pts',(-2.57923722849636,48.8276021287986,10.));
#15508=CARTESIAN_POINT('Ctrl Pts',(-2.60961658325033,48.914363699605,10.));
#15509=CARTESIAN_POINT('Ctrl Pts',(-2.63549494599023,49.0025379497205,10.));
#15510=CARTESIAN_POINT('Ctrl Pts',(-2.65658848539868,49.0919119517006,10.));
#15511=CARTESIAN_POINT('Ctrl Pts',(-2.66032107555693,49.1077270557348,10.));
#15512=CARTESIAN_POINT('Ctrl Pts',(-2.66390370811112,49.1235797355961,10.));
#15513=CARTESIAN_POINT('Ctrl Pts',(-2.66733463762423,49.139468817129,10.));
#15514=CARTESIAN_POINT('Ctrl Pts',(-2.68744534109363,49.2326041047786,10.));
#15515=CARTESIAN_POINT('Ctrl Pts',(-2.70234787596852,49.3269911317428,10.));
#15516=CARTESIAN_POINT('Ctrl Pts',(-2.7121207670544,49.422220824992,10.));
#15517=CARTESIAN_POINT('Ctrl Pts',(-2.71539839184387,49.4541588871832,10.));
#15518=CARTESIAN_POINT('Ctrl Pts',(-2.71809862149407,49.4861916106476,10.));
#15519=CARTESIAN_POINT('Ctrl Pts',(-2.72022319348791,49.5183030945014,10.));
#15520=CARTESIAN_POINT('Ctrl Pts',(-2.721411705215,49.5362666538656,10.));
#15521=CARTESIAN_POINT('Ctrl Pts',(-2.72242005876359,49.5542548554015,10.));
#15522=CARTESIAN_POINT('Ctrl Pts',(-2.72324847895075,49.5722648704493,10.));
#15523=CARTESIAN_POINT('Ctrl Pts',(-2.72382264730573,49.5847474015046,10.));
#15524=CARTESIAN_POINT('Ctrl Pts',(-2.72431026565451,49.5972388825475,10.));
#15525=CARTESIAN_POINT('Ctrl Pts',(-2.72471128394146,49.6097288907187,10.));
#15526=CARTESIAN_POINT('Ctrl Pts',(-2.72770346772776,49.7029226456101,10.));
#15527=CARTESIAN_POINT('Ctrl Pts',(-2.72588593808555,49.7961815023849,10.));
#15528=CARTESIAN_POINT('Ctrl Pts',(-2.71939783159665,49.8891301579573,10.));
#15529=CARTESIAN_POINT('Ctrl Pts',(-2.71289677354566,49.9822643576922,10.));
#15530=CARTESIAN_POINT('Ctrl Pts',(-2.70170608968587,50.0750880985227,10.));
#15531=CARTESIAN_POINT('Ctrl Pts',(-2.68591470530057,50.1672118275468,10.));
#15532=CARTESIAN_POINT('Ctrl Pts',(-2.67034661567951,50.258032900271,10.));
#15533=CARTESIAN_POINT('Ctrl Pts',(-2.65030654814482,50.3481744652969,10.));
#15534=CARTESIAN_POINT('Ctrl Pts',(-2.62583666370597,50.4372381109382,10.));
#15535=CARTESIAN_POINT('Ctrl Pts',(-2.61632323783499,50.4718643631678,10.));
#15536=CARTESIAN_POINT('Ctrl Pts',(-2.60613981410898,50.5063273483527,10.));
#15537=CARTESIAN_POINT('Ctrl Pts',(-2.59528730377686,50.540602191635,10.));
#15538=CARTESIAN_POINT('Ctrl Pts',(-2.58948288707972,50.5589339385351,10.));
#15539=CARTESIAN_POINT('Ctrl Pts',(-2.58348705736666,50.5772118500355,10.));
#15540=CARTESIAN_POINT('Ctrl Pts',(-2.57729985835685,50.5954320059774,10.));
#15541=CARTESIAN_POINT('Ctrl Pts',(-2.5718499952794,50.6114808440665,10.));
#15542=CARTESIAN_POINT('Ctrl Pts',(-2.56625117625606,50.6274859495329,10.));
#15543=CARTESIAN_POINT('Ctrl Pts',(-2.56050955613592,50.6434282233615,10.));
#15544=CARTESIAN_POINT('Ctrl Pts',(-2.52808295054336,50.733464452661,10.));
#15545=CARTESIAN_POINT('Ctrl Pts',(-2.49106530982848,50.8216219280263,10.));
#15546=CARTESIAN_POINT('Ctrl Pts',(-2.44952970456379,50.9074558899223,10.));
#15547=CARTESIAN_POINT('Ctrl Pts',(-2.41837800061528,50.9718313613443,10.));
#15548=CARTESIAN_POINT('Ctrl Pts',(-2.38468379325917,51.034899319489,10.));
#15549=CARTESIAN_POINT('Ctrl Pts',(-2.34846054129087,51.0964549719667,10.));
#15550=CARTESIAN_POINT('Ctrl Pts',(-2.33352933951851,51.1218281733618,10.));
#15551=CARTESIAN_POINT('Ctrl Pts',(-2.31816826890919,51.1469442216261,10.));
#15552=CARTESIAN_POINT('Ctrl Pts',(-2.30237761435193,51.1717878682362,10.));
#15553=CARTESIAN_POINT('Ctrl Pts',(-2.29294420526028,51.1866295760927,10.));
#15554=CARTESIAN_POINT('Ctrl Pts',(-2.28336215805488,51.2013666481012,10.));
#15555=CARTESIAN_POINT('Ctrl Pts',(-2.27363351537069,51.2159937552642,10.));
#15556=CARTESIAN_POINT('Ctrl Pts',(-2.22610549637866,51.2874525856076,10.));
#15557=CARTESIAN_POINT('Ctrl Pts',(-2.17506897708167,51.3563092144139,10.));
#15558=CARTESIAN_POINT('Ctrl Pts',(-2.12055836507602,51.422210815454,10.));
#15559=CARTESIAN_POINT('Ctrl Pts',(-2.06896996837888,51.484579550868,10.));
#15560=CARTESIAN_POINT('Ctrl Pts',(-2.01426948381755,51.5443018134259,10.));
#15561=CARTESIAN_POINT('Ctrl Pts',(-1.95646228443515,51.6010426460372,10.));
#15562=CARTESIAN_POINT('Ctrl Pts',(-1.94349623175226,51.6137695145375,10.));
#15563=CARTESIAN_POINT('Ctrl Pts',(-1.93037379547304,51.6263462293885,10.));
#15564=CARTESIAN_POINT('Ctrl Pts',(-1.91709820558804,51.6387714616175,10.));
#15565=CARTESIAN_POINT('Origin',(0.,50.,10.));
#15566=CARTESIAN_POINT('',(-6.,50.,10.));
#15567=CARTESIAN_POINT('Origin',(0.,50.,10.));
#15568=CARTESIAN_POINT('Origin',(0.,50.,5.));
#15569=CARTESIAN_POINT('Origin',(-15.,0.,2.));
#15570=CARTESIAN_POINT('',(-18.,3.67394039744206E-16,4.));
#15571=CARTESIAN_POINT('Origin',(-15.,0.,4.));
#15572=CARTESIAN_POINT('',(-18.,3.67394039744206E-16,0.));
#15573=CARTESIAN_POINT('',(-18.,3.67394039744206E-16,2.));
#15574=CARTESIAN_POINT('Origin',(-15.,0.,0.));
#15575=CARTESIAN_POINT('Origin',(15.,0.,2.));
#15576=CARTESIAN_POINT('',(12.,3.67394039744206E-16,4.));
#15577=CARTESIAN_POINT('Origin',(15.,0.,4.));
#15578=CARTESIAN_POINT('',(12.,3.67394039744206E-16,0.));
#15579=CARTESIAN_POINT('',(12.,3.67394039744206E-16,2.));
#15580=CARTESIAN_POINT('Origin',(15.,0.,0.));
#15581=CARTESIAN_POINT('Origin',(0.,0.,2.));
#15582=CARTESIAN_POINT('',(-5.,6.12323399573677E-16,4.));
#15583=CARTESIAN_POINT('Origin',(0.,0.,4.));
#15584=CARTESIAN_POINT('',(-5.,6.12323399573677E-16,0.));
#15585=CARTESIAN_POINT('',(-5.,6.12323399573677E-16,2.));
#15586=CARTESIAN_POINT('Origin',(0.,0.,0.));
#15587=CARTESIAN_POINT('Origin',(0.,50.,0.));
#15588=CARTESIAN_POINT('',(-6.,50.,4.));
#15589=CARTESIAN_POINT('',(-6.,50.,0.));
#15590=CARTESIAN_POINT('Origin',(0.,50.,4.));
#15591=CARTESIAN_POINT('Origin',(0.,50.,0.));
#15592=CARTESIAN_POINT('',(10.,50.,0.));
#15593=CARTESIAN_POINT('',(10.,50.,4.));
#15594=CARTESIAN_POINT('',(10.,50.,0.));
#15595=CARTESIAN_POINT('',(-10.,50.,0.));
#15596=CARTESIAN_POINT('Origin',(0.,50.,0.));
#15597=CARTESIAN_POINT('',(-10.,50.,4.));
#15598=CARTESIAN_POINT('',(-10.,50.,0.));
#15599=CARTESIAN_POINT('Origin',(0.,50.,4.));
#15600=CARTESIAN_POINT('Origin',(0.,0.,4.));
#15601=CARTESIAN_POINT('',(-10.,6.,4.));
#15602=CARTESIAN_POINT('',(-10.,50.,4.));
#15603=CARTESIAN_POINT('',(-15.,6.,4.));
#15604=CARTESIAN_POINT('',(15.,6.,4.));
#15605=CARTESIAN_POINT('',(-15.,-6.,4.));
#15606=CARTESIAN_POINT('Origin',(-15.,0.,4.));
#15607=CARTESIAN_POINT('',(-5.29150262212918,-6.,4.));
#15608=CARTESIAN_POINT('',(-15.,-6.,4.));
#15609=CARTESIAN_POINT('',(5.29150262212918,-6.,4.));
#15610=CARTESIAN_POINT('Origin',(0.,0.,4.));
#15611=CARTESIAN_POINT('',(15.,-6.,4.));
#15612=CARTESIAN_POINT('',(-15.,-6.,4.));
#15613=CARTESIAN_POINT('',(15.,6.,4.));
#15614=CARTESIAN_POINT('Origin',(15.,0.,4.));
#15615=CARTESIAN_POINT('',(10.,6.,4.));
#15616=CARTESIAN_POINT('',(15.,6.,4.));
#15617=CARTESIAN_POINT('',(10.,0.,4.));
#15618=CARTESIAN_POINT('Origin',(10.,0.,0.));
#15619=CARTESIAN_POINT('',(10.,6.,0.));
#15620=CARTESIAN_POINT('',(10.,6.,0.));
#15621=CARTESIAN_POINT('',(10.,0.,0.));
#15622=CARTESIAN_POINT('Origin',(-10.,50.,0.));
#15623=CARTESIAN_POINT('',(-10.,6.,0.));
#15624=CARTESIAN_POINT('',(-10.,6.,0.));
#15625=CARTESIAN_POINT('',(-10.,50.,0.));
#15626=CARTESIAN_POINT('Origin',(15.,6.,0.));
#15627=CARTESIAN_POINT('',(-15.,6.,0.));
#15628=CARTESIAN_POINT('',(15.,6.,0.));
#15629=CARTESIAN_POINT('',(-15.,6.,0.));
#15630=CARTESIAN_POINT('Origin',(0.,0.,0.));
#15631=CARTESIAN_POINT('',(15.,6.,0.));
#15632=CARTESIAN_POINT('',(15.,6.,0.));
#15633=CARTESIAN_POINT('',(15.,-6.,0.));
#15634=CARTESIAN_POINT('Origin',(15.,0.,0.));
#15635=CARTESIAN_POINT('',(5.29150262212918,-6.,0.));
#15636=CARTESIAN_POINT('',(-15.,-6.,0.));
#15637=CARTESIAN_POINT('',(-5.29150262212918,-6.,0.));
#15638=CARTESIAN_POINT('Origin',(0.,0.,0.));
#15639=CARTESIAN_POINT('',(-15.,-6.,0.));
#15640=CARTESIAN_POINT('',(-15.,-6.,0.));
#15641=CARTESIAN_POINT('Origin',(-15.,0.,0.));
#15642=CARTESIAN_POINT('Origin',(0.,0.,0.));
#15643=CARTESIAN_POINT('',(5.29150262212918,-6.,0.));
#15644=CARTESIAN_POINT('',(-5.29150262212918,-6.,0.));
#15645=CARTESIAN_POINT('Origin',(15.,6.,0.));
#15646=CARTESIAN_POINT('',(15.,6.,0.));
#15647=CARTESIAN_POINT('Origin',(-15.,-6.,0.));
#15648=CARTESIAN_POINT('',(-15.,-6.,0.));
#15649=CARTESIAN_POINT('Origin',(15.,0.,0.));
#15650=CARTESIAN_POINT('',(15.,-6.,0.));
#15651=CARTESIAN_POINT('Origin',(-15.,-6.,0.));
#15652=CARTESIAN_POINT('Origin',(-15.,0.,0.));
#15653=CARTESIAN_POINT('',(0.,0.,0.));
#15654=CARTESIAN_POINT('Origin',(-1.,0.,-37.));
#15655=CARTESIAN_POINT('',(1.,4.,-37.));
#15656=CARTESIAN_POINT('',(1.,-4.,-37.));
#15657=CARTESIAN_POINT('',(1.,0.,-37.));
#15658=CARTESIAN_POINT('',(-1.,-4.,-37.));
#15659=CARTESIAN_POINT('',(-3.5,-4.,-37.));
#15660=CARTESIAN_POINT('',(-1.,4.,-37.));
#15661=CARTESIAN_POINT('',(-1.,0.,-37.));
#15662=CARTESIAN_POINT('',(2.5,4.,-37.));
#15663=CARTESIAN_POINT('Origin',(-1.,0.,-40.));
#15664=CARTESIAN_POINT('',(-1.,-4.,-43.));
#15665=CARTESIAN_POINT('Origin',(-1.,-4.,-40.));
#15666=CARTESIAN_POINT('',(-1.,4.,-43.));
#15667=CARTESIAN_POINT('',(-1.,0.,-43.));
#15668=CARTESIAN_POINT('Origin',(-1.,4.,-40.));
#15669=CARTESIAN_POINT('Origin',(1.,0.,-43.));
#15670=CARTESIAN_POINT('',(1.,-4.,-43.));
#15671=CARTESIAN_POINT('',(-2.5,-4.,-43.));
#15672=CARTESIAN_POINT('',(1.,4.,-43.));
#15673=CARTESIAN_POINT('',(1.,0.,-43.));
#15674=CARTESIAN_POINT('',(3.5,4.,-43.));
#15675=CARTESIAN_POINT('Origin',(1.,0.,-40.));
#15676=CARTESIAN_POINT('Origin',(1.,-4.,-40.));
#15677=CARTESIAN_POINT('Origin',(1.,4.,-40.));
#15678=CARTESIAN_POINT('Origin',(0.,0.,-6.));
#15679=CARTESIAN_POINT('',(-2.,-4.,-6.));
#15680=CARTESIAN_POINT('',(2.,-4.,-6.));
#15681=CARTESIAN_POINT('',(-4.,-4.,-6.));
#15682=CARTESIAN_POINT('',(2.,-6.,-6.));
#15683=CARTESIAN_POINT('',(2.,-6.,-6.));
#15684=CARTESIAN_POINT('',(-2.,-6.,-6.));
#15685=CARTESIAN_POINT('',(-2.,-6.,-6.));
#15686=CARTESIAN_POINT('',(-2.,6.,-6.));
#15687=CARTESIAN_POINT('Origin',(0.,0.,-6.));
#15688=CARTESIAN_POINT('',(2.,4.,-6.));
#15689=CARTESIAN_POINT('',(-2.,4.,-6.));
#15690=CARTESIAN_POINT('',(4.,4.,-6.));
#15691=CARTESIAN_POINT('',(-2.,6.,-6.));
#15692=CARTESIAN_POINT('',(-2.,6.,-6.));
#15693=CARTESIAN_POINT('',(2.,6.,-6.));
#15694=CARTESIAN_POINT('',(2.,6.,-6.));
#15695=CARTESIAN_POINT('',(2.,-6.,-6.));
#15696=CARTESIAN_POINT('Origin',(2.,6.,-6.));
#15697=CARTESIAN_POINT('',(-2.,6.,2.));
#15698=CARTESIAN_POINT('',(-2.,6.,-6.));
#15699=CARTESIAN_POINT('',(2.,6.,2.));
#15700=CARTESIAN_POINT('',(2.,6.,2.));
#15701=CARTESIAN_POINT('',(2.,6.,-6.));
#15702=CARTESIAN_POINT('Origin',(2.,-6.,-6.));
#15703=CARTESIAN_POINT('',(2.,-3.,-6.));
#15704=CARTESIAN_POINT('',(2.,-6.,2.));
#15705=CARTESIAN_POINT('',(2.,-6.,2.));
#15706=CARTESIAN_POINT('',(2.,-6.,-6.));
#15707=CARTESIAN_POINT('Origin',(-2.,-6.,-6.));
#15708=CARTESIAN_POINT('',(-2.,-6.,2.));
#15709=CARTESIAN_POINT('',(-2.,-6.,2.));
#15710=CARTESIAN_POINT('',(-2.,-6.,-6.));
#15711=CARTESIAN_POINT('Origin',(-2.,6.,-6.));
#15712=CARTESIAN_POINT('',(-2.,3.,-6.));
#15713=CARTESIAN_POINT('',(-2.,6.,2.));
#15714=CARTESIAN_POINT('Origin',(0.,0.,2.));
#15715=CARTESIAN_POINT('Origin',(0.,0.,-6.));
#15716=CARTESIAN_POINT('',(-4.,4.,-6.));
#15717=CARTESIAN_POINT('',(4.,4.,-6.));
#15718=CARTESIAN_POINT('',(-4.,-4.,-6.));
#15719=CARTESIAN_POINT('',(-4.,4.,-6.));
#15720=CARTESIAN_POINT('',(-4.,-4.,-6.));
#15721=CARTESIAN_POINT('Origin',(0.,0.,-6.));
#15722=CARTESIAN_POINT('',(4.,-4.,-6.));
#15723=CARTESIAN_POINT('',(-4.,-4.,-6.));
#15724=CARTESIAN_POINT('',(4.,4.,-6.));
#15725=CARTESIAN_POINT('',(4.,-4.,-6.));
#15726=CARTESIAN_POINT('',(4.,4.,-6.));
#15727=CARTESIAN_POINT('Origin',(4.,-4.,-34.));
#15728=CARTESIAN_POINT('',(4.,4.,-34.));
#15729=CARTESIAN_POINT('',(4.,-4.,-34.));
#15730=CARTESIAN_POINT('',(4.,-2.,-34.));
#15731=CARTESIAN_POINT('',(4.,4.,-34.));
#15732=CARTESIAN_POINT('',(4.,-4.,-34.));
#15733=CARTESIAN_POINT('Origin',(-4.,4.,-34.));
#15734=CARTESIAN_POINT('',(-4.,-4.,-34.));
#15735=CARTESIAN_POINT('',(-4.,4.,-34.));
#15736=CARTESIAN_POINT('',(-4.,2.,-34.));
#15737=CARTESIAN_POINT('',(-4.,-4.,-34.));
#15738=CARTESIAN_POINT('',(-4.,4.,-34.));
#15739=CARTESIAN_POINT('Origin',(0.,0.,-34.));
#15740=CARTESIAN_POINT('',(-6.,4.,-34.));
#15741=CARTESIAN_POINT('',(6.,4.,-34.));
#15742=CARTESIAN_POINT('',(-6.,-4.,-34.));
#15743=CARTESIAN_POINT('',(-6.,4.,-34.));
#15744=CARTESIAN_POINT('',(-6.,-4.,-34.));
#15745=CARTESIAN_POINT('Origin',(6.,4.,-46.));
#15746=CARTESIAN_POINT('',(6.,4.,-46.));
#15747=CARTESIAN_POINT('',(-6.,4.,-46.));
#15748=CARTESIAN_POINT('',(6.,4.,-46.));
#15749=CARTESIAN_POINT('',(-6.,4.,-46.));
#15750=CARTESIAN_POINT('',(6.,4.,-34.));
#15751=CARTESIAN_POINT('',(6.,4.,-34.));
#15752=CARTESIAN_POINT('',(6.,4.,-46.));
#15753=CARTESIAN_POINT('Origin',(6.,-4.,-46.));
#15754=CARTESIAN_POINT('',(6.,-4.,-46.));
#15755=CARTESIAN_POINT('',(6.,-4.,-46.));
#15756=CARTESIAN_POINT('',(6.,-4.,-34.));
#15757=CARTESIAN_POINT('',(6.,-4.,-34.));
#15758=CARTESIAN_POINT('',(6.,-4.,-46.));
#15759=CARTESIAN_POINT('Origin',(-6.,-4.,-46.));
#15760=CARTESIAN_POINT('',(-6.,-4.,-46.));
#15761=CARTESIAN_POINT('',(-6.,-4.,-46.));
#15762=CARTESIAN_POINT('',(-6.,-4.,-34.));
#15763=CARTESIAN_POINT('',(-6.,-4.,-46.));
#15764=CARTESIAN_POINT('Origin',(-6.,4.,-46.));
#15765=CARTESIAN_POINT('',(-6.,4.,-46.));
#15766=CARTESIAN_POINT('Origin',(0.,0.,-34.));
#15767=CARTESIAN_POINT('Origin',(0.,0.,-46.));
#15768=CARTESIAN_POINT('',(0.,0.,0.));
#15769=CARTESIAN_POINT('Origin',(0.,0.,13.5));
#15770=CARTESIAN_POINT('',(-2.,-2.44929359829471E-16,13.));
#15771=CARTESIAN_POINT('Origin',(0.,0.,13.));
#15772=CARTESIAN_POINT('',(-2.,-2.44929359829471E-16,14.));
#15773=CARTESIAN_POINT('',(-2.,-2.44929359829471E-16,13.5));
#15774=CARTESIAN_POINT('Origin',(0.,0.,14.));
#15775=CARTESIAN_POINT('Origin',(6.,0.,13.));
#15776=CARTESIAN_POINT('',(-3.,3.67394039744206E-16,13.));
#15777=CARTESIAN_POINT('Origin',(0.,0.,13.));
#15778=CARTESIAN_POINT('Origin',(2.,0.,14.));
#15779=CARTESIAN_POINT('',(-3.,-3.67394039744206E-16,14.));
#15780=CARTESIAN_POINT('Origin',(0.,0.,14.));
#15781=CARTESIAN_POINT('Origin',(0.,0.,0.));
#15782=CARTESIAN_POINT('',(-3.,-3.67394039744206E-16,15.));
#15783=CARTESIAN_POINT('Origin',(0.,0.,15.));
#15784=CARTESIAN_POINT('',(-3.,-3.67394039744206E-16,0.));
#15785=CARTESIAN_POINT('Origin',(0.,0.,0.));
#15786=CARTESIAN_POINT('',(-5.,-6.12323399573677E-16,0.));
#15787=CARTESIAN_POINT('Origin',(0.,0.,0.));
#15788=CARTESIAN_POINT('',(-3.,-3.67394039744206E-16,0.));
#15789=CARTESIAN_POINT('Origin',(0.,0.,0.));
#15790=CARTESIAN_POINT('Origin',(0.,0.,-2.));
#15791=CARTESIAN_POINT('',(-5.,-6.12323399573677E-16,-2.));
#15792=CARTESIAN_POINT('',(-5.,-6.12323399573677E-16,-2.));
#15793=CARTESIAN_POINT('Origin',(0.,0.,-2.));
#15794=CARTESIAN_POINT('Origin',(0.,0.,-2.));
#15795=CARTESIAN_POINT('Origin',(0.,0.,0.));
#15796=CARTESIAN_POINT('',(-3.,-3.67394039744206E-16,0.));
#15797=CARTESIAN_POINT('Origin',(0.,0.,15.));
#15798=CARTESIAN_POINT('',(0.,0.,0.));
#15799=CARTESIAN_POINT('Origin',(0.,0.,30.5));
#15800=CARTESIAN_POINT('',(-3.,-3.67394039744206E-16,30.));
#15801=CARTESIAN_POINT('Origin',(0.,0.,30.));
#15802=CARTESIAN_POINT('',(-3.,-3.67394039744206E-16,31.));
#15803=CARTESIAN_POINT('',(-3.,-3.67394039744206E-16,30.5));
#15804=CARTESIAN_POINT('Origin',(0.,0.,31.));
#15805=CARTESIAN_POINT('Origin',(7.,0.,30.));
#15806=CARTESIAN_POINT('',(-4.,4.89858719658941E-16,30.));
#15807=CARTESIAN_POINT('Origin',(0.,0.,30.));
#15808=CARTESIAN_POINT('Origin',(3.,0.,31.));
#15809=CARTESIAN_POINT('',(-4.,-4.89858719658941E-16,31.));
#15810=CARTESIAN_POINT('Origin',(0.,0.,31.));
#15811=CARTESIAN_POINT('Origin',(0.,0.,0.));
#15812=CARTESIAN_POINT('',(-4.,-4.89858719658941E-16,32.));
#15813=CARTESIAN_POINT('Origin',(0.,0.,32.));
#15814=CARTESIAN_POINT('',(-4.,-4.89858719658941E-16,0.));
#15815=CARTESIAN_POINT('Origin',(0.,0.,0.));
#15816=CARTESIAN_POINT('',(-7.,-8.57252759403147E-16,0.));
#15817=CARTESIAN_POINT('Origin',(0.,0.,0.));
#15818=CARTESIAN_POINT('',(-4.,-4.89858719658941E-16,0.));
#15819=CARTESIAN_POINT('Origin',(0.,0.,0.));
#15820=CARTESIAN_POINT('Origin',(0.,0.,-3.));
#15821=CARTESIAN_POINT('',(-7.,-8.57252759403147E-16,-3.));
#15822=CARTESIAN_POINT('',(-7.,-8.57252759403147E-16,-3.));
#15823=CARTESIAN_POINT('Origin',(0.,0.,-3.));
#15824=CARTESIAN_POINT('Origin',(0.,0.,-3.));
#15825=CARTESIAN_POINT('Origin',(0.,0.,0.));
#15826=CARTESIAN_POINT('',(-4.,-4.89858719658941E-16,0.));
#15827=CARTESIAN_POINT('Origin',(0.,0.,32.));
#15828=CARTESIAN_POINT('',(0.,0.,0.));
#15829=CARTESIAN_POINT('Origin',(0.,0.,0.));
#15830=CARTESIAN_POINT('',(-3.,-3.67394039744206E-16,1.));
#15831=CARTESIAN_POINT('Origin',(0.,0.,1.));
#15832=CARTESIAN_POINT('',(-3.,-3.67394039744206E-16,0.));
#15833=CARTESIAN_POINT('',(-3.,-3.67394039744206E-16,0.));
#15834=CARTESIAN_POINT('Origin',(0.,0.,0.));
#15835=CARTESIAN_POINT('Origin',(0.,0.,0.));
#15836=CARTESIAN_POINT('',(-5.,-6.12323399573677E-16,1.));
#15837=CARTESIAN_POINT('Origin',(0.,0.,1.));
#15838=CARTESIAN_POINT('',(-5.,-6.12323399573677E-16,0.));
#15839=CARTESIAN_POINT('',(-5.,-6.12323399573677E-16,0.));
#15840=CARTESIAN_POINT('Origin',(0.,0.,0.));
#15841=CARTESIAN_POINT('Origin',(0.,0.,1.));
#15842=CARTESIAN_POINT('Origin',(0.,0.,0.));
#15843=CARTESIAN_POINT('',(0.,0.,0.));
#15844=CARTESIAN_POINT('Origin',(-1.,0.,1.));
#15845=CARTESIAN_POINT('',(-1.,1.73205080756888,0.));
#15846=CARTESIAN_POINT('',(-1.,1.73205080756888,1.));
#15847=CARTESIAN_POINT('',(-1.,1.73205080756888,0.));
#15848=CARTESIAN_POINT('',(-1.,4.89897948556636,0.));
#15849=CARTESIAN_POINT('',(-1.,0.,0.));
#15850=CARTESIAN_POINT('',(-1.,4.89897948556636,1.));
#15851=CARTESIAN_POINT('',(-1.,4.89897948556636,0.));
#15852=CARTESIAN_POINT('',(-1.,0.,1.));
#15853=CARTESIAN_POINT('Origin',(1.,10.,1.));
#15854=CARTESIAN_POINT('',(1.,1.73205080756888,1.));
#15855=CARTESIAN_POINT('',(1.,1.73205080756888,0.));
#15856=CARTESIAN_POINT('',(1.,1.73205080756888,0.));
#15857=CARTESIAN_POINT('',(1.,4.89897948556636,1.));
#15858=CARTESIAN_POINT('',(1.,5.,1.));
#15859=CARTESIAN_POINT('',(1.,4.89897948556636,0.));
#15860=CARTESIAN_POINT('',(1.,4.89897948556636,0.));
#15861=CARTESIAN_POINT('',(1.,5.,0.));
#15862=CARTESIAN_POINT('Origin',(0.,0.,0.));
#15863=CARTESIAN_POINT('Origin',(0.,0.,0.));
#15864=CARTESIAN_POINT('Origin',(0.,0.,0.));
#15865=CARTESIAN_POINT('Origin',(0.,0.,0.));
#15866=CARTESIAN_POINT('Origin',(0.,0.,1.));
#15867=CARTESIAN_POINT('Origin',(0.,0.,0.));
#15868=CARTESIAN_POINT('Origin',(0.,0.,1.));
#15869=CARTESIAN_POINT('Origin',(0.,0.,1.));
#15870=CARTESIAN_POINT('',(0.,0.,0.));
#15871=CARTESIAN_POINT('Origin',(0.,0.,0.));
#15872=CARTESIAN_POINT('',(-4.,-4.89858719658941E-16,4.));
#15873=CARTESIAN_POINT('Origin',(0.,0.,4.));
#15874=CARTESIAN_POINT('',(-4.,-4.89858719658941E-16,0.));
#15875=CARTESIAN_POINT('',(-4.,-4.89858719658941E-16,0.));
#15876=CARTESIAN_POINT('Origin',(0.,0.,0.));
#15877=CARTESIAN_POINT('Origin',(0.,0.,0.));
#15878=CARTESIAN_POINT('',(-5.,-6.12323399573677E-16,4.));
#15879=CARTESIAN_POINT('Origin',(0.,0.,4.));
#15880=CARTESIAN_POINT('',(-5.,-6.12323399573677E-16,0.));
#15881=CARTESIAN_POINT('',(-5.,-6.12323399573677E-16,0.));
#15882=CARTESIAN_POINT('Origin',(0.,0.,0.));
#15883=CARTESIAN_POINT('Origin',(0.,0.,4.));
#15884=CARTESIAN_POINT('Origin',(0.,0.,0.));
#15885=CARTESIAN_POINT('',(0.,0.,0.));
#15886=CARTESIAN_POINT('Origin',(0.,0.,0.));
#15887=CARTESIAN_POINT('',(-4.,-4.89858719658941E-16,2.));
#15888=CARTESIAN_POINT('Origin',(0.,0.,2.));
#15889=CARTESIAN_POINT('',(-4.,-4.89858719658941E-16,0.));
#15890=CARTESIAN_POINT('',(-4.,-4.89858719658941E-16,0.));
#15891=CARTESIAN_POINT('Origin',(0.,0.,0.));
#15892=CARTESIAN_POINT('Origin',(0.,0.,0.));
#15893=CARTESIAN_POINT('',(-7.,-8.57252759403147E-16,2.));
#15894=CARTESIAN_POINT('Origin',(0.,0.,2.));
#15895=CARTESIAN_POINT('',(-7.,-8.57252759403147E-16,0.));
#15896=CARTESIAN_POINT('',(-7.,-8.57252759403147E-16,0.));
#15897=CARTESIAN_POINT('Origin',(0.,0.,0.));
#15898=CARTESIAN_POINT('Origin',(0.,0.,2.));
#15899=CARTESIAN_POINT('Origin',(0.,0.,0.));
#15900=CARTESIAN_POINT('',(0.,0.,0.));
#15901=CARTESIAN_POINT('Origin',(0.,0.,0.));
#15902=CARTESIAN_POINT('',(-4.,-4.89858719658941E-16,12.));
#15903=CARTESIAN_POINT('Origin',(0.,0.,12.));
#15904=CARTESIAN_POINT('',(-4.,-4.89858719658941E-16,0.));
#15905=CARTESIAN_POINT('',(-4.,-4.89858719658941E-16,0.));
#15906=CARTESIAN_POINT('Origin',(0.,0.,0.));
#15907=CARTESIAN_POINT('Origin',(0.,0.,0.));
#15908=CARTESIAN_POINT('',(-8.,-9.79717439317883E-16,12.));
#15909=CARTESIAN_POINT('Origin',(0.,0.,12.));
#15910=CARTESIAN_POINT('',(-8.,-9.79717439317883E-16,0.));
#15911=CARTESIAN_POINT('',(-8.,-9.79717439317883E-16,0.));
#15912=CARTESIAN_POINT('Origin',(0.,0.,0.));
#15913=CARTESIAN_POINT('Origin',(0.,0.,12.));
#15914=CARTESIAN_POINT('Origin',(0.,0.,0.));
#15915=CARTESIAN_POINT('',(0.,0.,0.));
#15916=CARTESIAN_POINT('Origin',(-1.,0.,1.));
#15917=CARTESIAN_POINT('',(-1.,2.82842712474619,0.));
#15918=CARTESIAN_POINT('',(-1.,2.82842712474619,1.));
#15919=CARTESIAN_POINT('',(-1.,2.82842712474619,0.));
#15920=CARTESIAN_POINT('',(-1.,6.92820323027551,0.));
#15921=CARTESIAN_POINT('',(-1.,0.,0.));
#15922=CARTESIAN_POINT('',(-1.,6.92820323027551,1.));
#15923=CARTESIAN_POINT('',(-1.,6.92820323027551,0.));
#15924=CARTESIAN_POINT('',(-1.,0.,1.));
#15925=CARTESIAN_POINT('Origin',(1.,14.,1.));
#15926=CARTESIAN_POINT('',(1.,2.82842712474619,1.));
#15927=CARTESIAN_POINT('',(1.,2.82842712474619,0.));
#15928=CARTESIAN_POINT('',(1.,2.82842712474619,0.));
#15929=CARTESIAN_POINT('',(1.,6.92820323027551,1.));
#15930=CARTESIAN_POINT('',(1.,7.,1.));
#15931=CARTESIAN_POINT('',(1.,6.92820323027551,0.));
#15932=CARTESIAN_POINT('',(1.,6.92820323027551,0.));
#15933=CARTESIAN_POINT('',(1.,7.,0.));
#15934=CARTESIAN_POINT('Origin',(0.,0.,0.));
#15935=CARTESIAN_POINT('Origin',(0.,0.,0.));
#15936=CARTESIAN_POINT('Origin',(0.,0.,0.));
#15937=CARTESIAN_POINT('Origin',(0.,0.,0.));
#15938=CARTESIAN_POINT('Origin',(0.,0.,1.));
#15939=CARTESIAN_POINT('Origin',(0.,0.,0.));
#15940=CARTESIAN_POINT('Origin',(0.,0.,1.));
#15941=CARTESIAN_POINT('Origin',(0.,0.,1.));
#15942=CARTESIAN_POINT('',(0.,0.,0.));
#15943=CARTESIAN_POINT('Origin',(0.,0.,11.5));
#15944=CARTESIAN_POINT('',(-1.5,-1.83697019872103E-16,11.));
#15945=CARTESIAN_POINT('Origin',(0.,0.,11.));
#15946=CARTESIAN_POINT('',(-1.5,-1.83697019872103E-16,12.));
#15947=CARTESIAN_POINT('',(-1.5,-1.83697019872103E-16,11.5));
#15948=CARTESIAN_POINT('Origin',(0.,0.,12.));
#15949=CARTESIAN_POINT('Origin',(5.5,0.,11.));
#15950=CARTESIAN_POINT('',(-2.,2.44929359829471E-16,11.));
#15951=CARTESIAN_POINT('Origin',(0.,0.,11.));
#15952=CARTESIAN_POINT('Origin',(1.5,0.,12.));
#15953=CARTESIAN_POINT('',(-2.,-2.44929359829471E-16,12.));
#15954=CARTESIAN_POINT('Origin',(0.,0.,12.));
#15955=CARTESIAN_POINT('Origin',(0.,0.,0.));
#15956=CARTESIAN_POINT('',(-2.,-2.44929359829471E-16,13.));
#15957=CARTESIAN_POINT('Origin',(0.,0.,13.));
#15958=CARTESIAN_POINT('',(-2.,-2.44929359829471E-16,0.));
#15959=CARTESIAN_POINT('Origin',(0.,0.,0.));
#15960=CARTESIAN_POINT('',(-4.,-4.89858719658941E-16,0.));
#15961=CARTESIAN_POINT('Origin',(0.,0.,0.));
#15962=CARTESIAN_POINT('',(-2.,-2.44929359829471E-16,0.));
#15963=CARTESIAN_POINT('Origin',(0.,0.,0.));
#15964=CARTESIAN_POINT('Origin',(0.,0.,-2.));
#15965=CARTESIAN_POINT('',(-4.,-4.89858719658941E-16,-2.));
#15966=CARTESIAN_POINT('',(-4.,-4.89858719658941E-16,-2.));
#15967=CARTESIAN_POINT('Origin',(0.,0.,-2.));
#15968=CARTESIAN_POINT('Origin',(0.,0.,-2.));
#15969=CARTESIAN_POINT('Origin',(0.,0.,0.));
#15970=CARTESIAN_POINT('',(-2.,-2.44929359829471E-16,0.));
#15971=CARTESIAN_POINT('Origin',(0.,0.,13.));
#15972=CARTESIAN_POINT('',(0.,0.,0.));
#15973=CARTESIAN_POINT('Origin',(0.,0.,0.));
#15974=CARTESIAN_POINT('',(-2.,-2.44929359829471E-16,2.));
#15975=CARTESIAN_POINT('Origin',(0.,0.,2.));
#15976=CARTESIAN_POINT('',(-2.,-2.44929359829471E-16,0.));
#15977=CARTESIAN_POINT('',(-2.,-2.44929359829471E-16,0.));
#15978=CARTESIAN_POINT('Origin',(0.,0.,0.));
#15979=CARTESIAN_POINT('Origin',(0.,0.,0.));
#15980=CARTESIAN_POINT('',(-4.,-4.89858719658941E-16,2.));
#15981=CARTESIAN_POINT('Origin',(0.,0.,2.));
#15982=CARTESIAN_POINT('',(-4.,-4.89858719658941E-16,0.));
#15983=CARTESIAN_POINT('',(-4.,-4.89858719658941E-16,0.));
#15984=CARTESIAN_POINT('Origin',(0.,0.,0.));
#15985=CARTESIAN_POINT('Origin',(0.,0.,2.));
#15986=CARTESIAN_POINT('Origin',(0.,0.,0.));
#15987=CARTESIAN_POINT('',(0.,0.,0.));
#15988=CARTESIAN_POINT('Origin',(0.,0.,0.));
#15989=CARTESIAN_POINT('',(-2.,-2.44929359829471E-16,1.));
#15990=CARTESIAN_POINT('Origin',(0.,0.,1.));
#15991=CARTESIAN_POINT('',(-2.,-2.44929359829471E-16,0.));
#15992=CARTESIAN_POINT('',(-2.,-2.44929359829471E-16,0.));
#15993=CARTESIAN_POINT('Origin',(0.,0.,0.));
#15994=CARTESIAN_POINT('Origin',(0.,0.,0.));
#15995=CARTESIAN_POINT('',(-4.,-4.89858719658941E-16,1.));
#15996=CARTESIAN_POINT('Origin',(0.,0.,1.));
#15997=CARTESIAN_POINT('',(-4.,-4.89858719658941E-16,0.));
#15998=CARTESIAN_POINT('',(-4.,-4.89858719658941E-16,0.));
#15999=CARTESIAN_POINT('Origin',(0.,0.,0.));
#16000=CARTESIAN_POINT('Origin',(0.,0.,1.));
#16001=CARTESIAN_POINT('Origin',(0.,0.,0.));
#16002=CARTESIAN_POINT('',(0.,0.,0.));
#16003=CARTESIAN_POINT('Origin',(-1.,0.,1.));
#16004=CARTESIAN_POINT('',(-1.,1.11803398874989,0.));
#16005=CARTESIAN_POINT('',(-1.,1.11803398874989,1.));
#16006=CARTESIAN_POINT('',(-1.,1.11803398874989,0.));
#16007=CARTESIAN_POINT('',(-1.,3.35410196624968,0.));
#16008=CARTESIAN_POINT('',(-1.,0.,0.));
#16009=CARTESIAN_POINT('',(-1.,3.35410196624968,1.));
#16010=CARTESIAN_POINT('',(-1.,3.35410196624968,0.));
#16011=CARTESIAN_POINT('',(-1.,0.,1.));
#16012=CARTESIAN_POINT('Origin',(1.,7.,1.));
#16013=CARTESIAN_POINT('',(1.,1.11803398874989,1.));
#16014=CARTESIAN_POINT('',(1.,1.11803398874989,0.));
#16015=CARTESIAN_POINT('',(1.,1.11803398874989,0.));
#16016=CARTESIAN_POINT('',(1.,3.35410196624968,1.));
#16017=CARTESIAN_POINT('',(1.,3.5,1.));
#16018=CARTESIAN_POINT('',(1.,3.35410196624968,0.));
#16019=CARTESIAN_POINT('',(1.,3.35410196624968,0.));
#16020=CARTESIAN_POINT('',(1.,3.5,0.));
#16021=CARTESIAN_POINT('Origin',(0.,0.,0.));
#16022=CARTESIAN_POINT('Origin',(0.,0.,0.));
#16023=CARTESIAN_POINT('Origin',(0.,0.,0.));
#16024=CARTESIAN_POINT('Origin',(0.,0.,0.));
#16025=CARTESIAN_POINT('Origin',(0.,0.,1.));
#16026=CARTESIAN_POINT('Origin',(0.,0.,0.));
#16027=CARTESIAN_POINT('Origin',(0.,0.,1.));
#16028=CARTESIAN_POINT('Origin',(0.,0.,1.));
#16029=CARTESIAN_POINT('',(0.,0.,0.));
#16030=CARTESIAN_POINT('Origin',(0.,0.,0.));
#16031=CARTESIAN_POINT('',(-4.,-4.89858719658941E-16,24.));
#16032=CARTESIAN_POINT('Origin',(0.,0.,24.));
#16033=CARTESIAN_POINT('',(-4.,-4.89858719658941E-16,0.));
#16034=CARTESIAN_POINT('',(-4.,-4.89858719658941E-16,0.));
#16035=CARTESIAN_POINT('Origin',(0.,0.,0.));
#16036=CARTESIAN_POINT('Origin',(0.,0.,0.));
#16037=CARTESIAN_POINT('',(-14.,1.71450551880629E-15,24.));
#16038=CARTESIAN_POINT('Origin',(0.,0.,24.));
#16039=CARTESIAN_POINT('',(-14.,1.71450551880629E-15,0.));
#16040=CARTESIAN_POINT('',(-14.,-1.71450551880629E-15,0.));
#16041=CARTESIAN_POINT('Origin',(0.,0.,0.));
#16042=CARTESIAN_POINT('Origin',(0.,0.,24.));
#16043=CARTESIAN_POINT('Origin',(0.,0.,0.));
#16044=CARTESIAN_POINT('',(0.,0.,0.));
#16045=CARTESIAN_POINT('Origin',(0.,0.,-9.84858989190502));
#16046=CARTESIAN_POINT('',(-2.37107105383284,-0.00233734150670739,-0.348589891905017));
#16047=CARTESIAN_POINT('',(-2.37527615294243,0.000221438259633937,-0.151410108094976));
#16048=CARTESIAN_POINT('',(-2.37175,-6.37235396393925E-14,-9.84858989190502));
#16049=CARTESIAN_POINT('',(1.37999758476545,-1.93379827794526,-6.88317517931686E-16));
#16050=CARTESIAN_POINT('Ctrl Pts',(-2.37107105383284,-0.00233734150670767,
-0.348589891905018));
#16051=CARTESIAN_POINT('Ctrl Pts',(-2.37291097660622,-0.207204195815191,
-0.334848170695028));
#16052=CARTESIAN_POINT('Ctrl Pts',(-2.25467011638231,-1.20079122991256,
-0.268056556211669));
#16053=CARTESIAN_POINT('Ctrl Pts',(-0.903419705864106,-2.62466631852008,
-0.15185992557666));
#16054=CARTESIAN_POINT('Ctrl Pts',(0.780890334042663,-2.35671012203314,
-0.0494050161516468));
#16055=CARTESIAN_POINT('Ctrl Pts',(1.38002164928817,-1.93382042716839,-8.34835672813838E-16));
#16056=CARTESIAN_POINT('',(-1.37702479013102,-1.93106208855765,0.));
#16057=CARTESIAN_POINT('Origin',(0.,0.,0.));
#16058=CARTESIAN_POINT('Ctrl Pts',(-2.37527615294243,0.000221438259633958,
-0.151410108094976));
#16059=CARTESIAN_POINT('Ctrl Pts',(-2.37262065161448,-0.747106869089609,
-0.100940072063317));
#16060=CARTESIAN_POINT('Ctrl Pts',(-1.98938888825771,-1.49439019245279,
-0.0504700360316578));
#16061=CARTESIAN_POINT('Ctrl Pts',(-1.37702479013101,-1.93106208855766,
1.11022302462516E-15));
#16062=CARTESIAN_POINT('Origin',(0.,0.,-9.84858989190502));
#16063=CARTESIAN_POINT('',(-2.36793723488955,0.000550897978577819,-1.34858989190502));
#16064=CARTESIAN_POINT('',(-2.37145569047744,-0.00220250059204397,-1.15141010809498));
#16065=CARTESIAN_POINT('',(-2.37175,-6.37235396393925E-14,-9.84858989190502));
#16066=CARTESIAN_POINT('Ctrl Pts',(-2.36793723488955,0.000550897978577602,
-1.34858989190502));
#16067=CARTESIAN_POINT('Ctrl Pts',(-2.3670439500601,-0.429886149741189,
-1.31981419700191));
#16068=CARTESIAN_POINT('Ctrl Pts',(-2.04853459375008,-1.65509205416319,
-1.23798860882543));
#16069=CARTESIAN_POINT('Ctrl Pts',(-0.0797314402530648,-2.80441033824713,
-1.10311312737558));
#16070=CARTESIAN_POINT('Ctrl Pts',(2.31673231987452,-1.58243891335296,-0.94396344755548));
#16071=CARTESIAN_POINT('Ctrl Pts',(2.58328372722621,1.0944611426978,-0.784813767735368));
#16072=CARTESIAN_POINT('Ctrl Pts',(0.47501218998366,2.76493134210758,-0.625664087915265));
#16073=CARTESIAN_POINT('Ctrl Pts',(-1.85037417679958,1.96916881916604,-0.480256129305143));
#16074=CARTESIAN_POINT('Ctrl Pts',(-2.36580795761266,0.583683975341639,
-0.387898063968396));
#16075=CARTESIAN_POINT('Ctrl Pts',(-2.37107105383284,-0.00233734150670767,
-0.348589891905018));
#16076=CARTESIAN_POINT('Ctrl Pts',(-2.37145569047744,-0.00220250059204391,
-1.15141010809498));
#16077=CARTESIAN_POINT('Ctrl Pts',(-2.37322010983073,-0.195721147004533,
-1.13842444706332));
#16078=CARTESIAN_POINT('Ctrl Pts',(-2.26301140298161,-1.17668930763203,
-1.07246482769833));
#16079=CARTESIAN_POINT('Ctrl Pts',(-0.902039595484687,-2.65503026080224,
-0.953531249999998));
#16080=CARTESIAN_POINT('Ctrl Pts',(1.74372732289156,-2.19643768378856,-0.794609375000001));
#16081=CARTESIAN_POINT('Ctrl Pts',(2.79043291661474,0.277087651255129,-0.635687499999998));
#16082=CARTESIAN_POINT('Ctrl Pts',(1.2788492724039,2.49472256946297,-0.476765624999999));
#16083=CARTESIAN_POINT('Ctrl Pts',(-1.4060176679778,2.42838470324144,-0.317843749999998));
#16084=CARTESIAN_POINT('Ctrl Pts',(-2.35757225025559,0.858781682425109,
-0.209391911031658));
#16085=CARTESIAN_POINT('Ctrl Pts',(-2.37540789782553,0.0372979328012767,
-0.15391403039665));
#16086=CARTESIAN_POINT('Ctrl Pts',(-2.37527615294243,0.000221438259633958,
-0.151410108094976));
#16087=CARTESIAN_POINT('Origin',(0.,0.,-9.84858989190502));
#16088=CARTESIAN_POINT('',(-2.37316232600006,0.00200347480865394,-2.34858989190502));
#16089=CARTESIAN_POINT('',(-2.36793686665521,0.000485999580435575,-2.15141010809498));
#16090=CARTESIAN_POINT('',(-2.37175,-6.37235396393925E-14,-9.84858989190502));
#16091=CARTESIAN_POINT('Ctrl Pts',(-2.37316232600006,0.00200347480865396,
-2.34858989190502));
#16092=CARTESIAN_POINT('Ctrl Pts',(-2.36728640162788,-0.649663311263526,
-2.30478022330879));
#16093=CARTESIAN_POINT('Ctrl Pts',(-1.75058100701069,-2.10021485722012,
-2.2079206614392));
#16094=CARTESIAN_POINT('Ctrl Pts',(0.707590769365126,-2.71486542435539,
-2.05801120629623));
#16095=CARTESIAN_POINT('Ctrl Pts',(2.66676527322589,-0.871519975440165,
-1.89886152647612));
#16096=CARTESIAN_POINT('Ctrl Pts',(2.17427552027739,1.77305104894897,-1.73971184665602));
#16097=CARTESIAN_POINT('Ctrl Pts',(-0.31711023351784,2.787580752663,-1.58056216683591));
#16098=CARTESIAN_POINT('Ctrl Pts',(-2.11921353689182,1.51931384506248,-1.45018818191891));
#16099=CARTESIAN_POINT('Ctrl Pts',(-2.36869077961624,0.363652964407927,
-1.37286409027528));
#16100=CARTESIAN_POINT('Ctrl Pts',(-2.36793723488955,0.000550897978577602,
-1.34858989190502));
#16101=CARTESIAN_POINT('Ctrl Pts',(-2.36793686665521,0.00048599958043568,
-2.15141010809498));
#16102=CARTESIAN_POINT('Ctrl Pts',(-2.36715767925933,-0.425457443633952,
-2.12293486372999));
#16103=CARTESIAN_POINT('Ctrl Pts',(-2.05372327229891,-1.64487463216302,
-2.04148566103166));
#16104=CARTESIAN_POINT('Ctrl Pts',(-0.0995709890729291,-2.80243276783242,
-1.9070625));
#16105=CARTESIAN_POINT('Ctrl Pts',(2.30202865838936,-1.60132637136797,-1.748140625));
#16106=CARTESIAN_POINT('Ctrl Pts',(2.59282079624265,1.06810673697464,-1.58921875));
#16107=CARTESIAN_POINT('Ctrl Pts',(0.506179573027947,2.75812167782342,-1.430296875));
#16108=CARTESIAN_POINT('Ctrl Pts',(-1.83618017076844,1.98774646240115,-1.28436066103166));
#16109=CARTESIAN_POINT('Ctrl Pts',(-2.36602230318261,0.59372258533879,-1.19139840539665));
#16110=CARTESIAN_POINT('Ctrl Pts',(-2.37145569047744,-0.00220250059204391,
-1.15141010809498));
#16111=CARTESIAN_POINT('Origin',(0.,0.,-9.84858989190502));
#16112=CARTESIAN_POINT('',(-2.37454708810461,-0.00146305467787407,-3.34858989190502));
#16113=CARTESIAN_POINT('',(-2.37324810841896,0.00196432295147285,-3.15141010809498));
#16114=CARTESIAN_POINT('',(-2.37175,-6.37235396393925E-14,-9.84858989190502));
#16115=CARTESIAN_POINT('Ctrl Pts',(-2.37454708810461,-0.00146305467787401,
-3.34858989190502));
#16116=CARTESIAN_POINT('Ctrl Pts',(-2.37516922171714,-0.0875139819792011,
-3.34279614288904));
#16117=CARTESIAN_POINT('Ctrl Pts',(-2.33179955053217,-0.960847969556608,
-3.2839525005997));
#16118=CARTESIAN_POINT('Ctrl Pts',(-1.24959461996354,-2.51191054810233,
-3.17205896503699));
#16119=CARTESIAN_POINT('Ctrl Pts',(1.43846132446067,-2.40873623914147,-3.01290928521687));
#16120=CARTESIAN_POINT('Ctrl Pts',(2.80408262807151,-0.0911150253769769,
-2.85375960539677));
#16121=CARTESIAN_POINT('Ctrl Pts',(1.59179933506719,2.3102719050862,-2.69460992557666));
#16122=CARTESIAN_POINT('Ctrl Pts',(-1.08388829677707,2.58773397497002,-2.53546024575656));
#16123=CARTESIAN_POINT('Ctrl Pts',(-2.30086818960063,1.0646887844646,-2.42012023453267));
#16124=CARTESIAN_POINT('Ctrl Pts',(-2.37440166113143,0.139451387812435,
-2.35783011658216));
#16125=CARTESIAN_POINT('Ctrl Pts',(-2.37316232600006,0.00200347480865396,
-2.34858989190502));
#16126=CARTESIAN_POINT('Ctrl Pts',(-2.37324810841896,0.00196432295147262,
-3.15141010809498));
#16127=CARTESIAN_POINT('Ctrl Pts',(-2.36742079101,-0.651949751271476,-3.10744528039665));
#16128=CARTESIAN_POINT('Ctrl Pts',(-1.74738494334323,-2.10348028265193,
-3.01050649436499));
#16129=CARTESIAN_POINT('Ctrl Pts',(0.71129970966804,-2.71249186414424,-2.86059375));
#16130=CARTESIAN_POINT('Ctrl Pts',(2.66552760696098,-0.870932032693957,
-2.701671875));
#16131=CARTESIAN_POINT('Ctrl Pts',(2.17564778740008,1.76921366782114,-2.54275));
#16132=CARTESIAN_POINT('Ctrl Pts',(-0.309153032213342,2.78710993733308,
-2.383828125));
#16133=CARTESIAN_POINT('Ctrl Pts',(-2.11605294401407,1.52493739017563,-2.25338149436499));
#16134=CARTESIAN_POINT('Ctrl Pts',(-2.36860724155681,0.366947001573718,
-2.17590882206332));
#16135=CARTESIAN_POINT('Ctrl Pts',(-2.36793686665521,0.00048599958043568,
-2.15141010809498));
#16136=CARTESIAN_POINT('Origin',(0.,0.,-9.84858989190502));
#16137=CARTESIAN_POINT('',(-2.36855400559966,-0.00132034435408072,-4.34858989190502));
#16138=CARTESIAN_POINT('',(-2.37427834230277,-0.00158579729887448,-4.15141010809498));
#16139=CARTESIAN_POINT('',(-2.37175,-6.37235396393925E-14,-9.84858989190502));
#16140=CARTESIAN_POINT('Ctrl Pts',(-2.36855400559966,-0.00132034435408088,
-4.34858989190502));
#16141=CARTESIAN_POINT('Ctrl Pts',(-2.37012134036242,-0.312665446856959,
-4.32776216919593));
#16142=CARTESIAN_POINT('Ctrl Pts',(-2.16801155330476,-1.41507745062122,
-4.25388455321346));
#16143=CARTESIAN_POINT('Ctrl Pts',(-0.497409040646124,-2.76111672375383,
-4.12695704395763));
#16144=CARTESIAN_POINT('Ctrl Pts',(2.05458518082845,-1.91046094844367,-3.96780736413752));
#16145=CARTESIAN_POINT('Ctrl Pts',(2.717717602526,0.69655748161016,-3.80865768431742));
#16146=CARTESIAN_POINT('Ctrl Pts',(0.882344250202438,2.66320294535576,-3.64950800449731));
#16147=CARTESIAN_POINT('Ctrl Pts',(-1.66785725130337,2.19899767883659,-3.49615207369318));
#16148=CARTESIAN_POINT('Ctrl Pts',(-2.36947271645676,0.700402874070681,
-3.39584603616241));
#16149=CARTESIAN_POINT('Ctrl Pts',(-2.37454708810461,-0.00146305467787401,
-3.34858989190502));
#16150=CARTESIAN_POINT('Ctrl Pts',(-2.37427834230277,-0.00158579729887398,
-4.15141010809498));
#16151=CARTESIAN_POINT('Ctrl Pts',(-2.3750191981319,-0.0978644702926246,
-4.14492965539666));
#16152=CARTESIAN_POINT('Ctrl Pts',(-2.3259543184558,-0.980404337668707,
-4.08547524436499));
#16153=CARTESIAN_POINT('Ctrl Pts',(-1.22000243857572,-2.52490668674665,
-3.973046875));
#16154=CARTESIAN_POINT('Ctrl Pts',(1.46196288604333,-2.39295303517309,-3.814125));
#16155=CARTESIAN_POINT('Ctrl Pts',(2.80340761681022,-0.0668241043267523,
-3.655203125));
#16156=CARTESIAN_POINT('Ctrl Pts',(1.57431810519612,2.32057799752537,-3.49628125));
#16157=CARTESIAN_POINT('Ctrl Pts',(-1.09831409983361,2.58016778763604,-3.337359375));
#16158=CARTESIAN_POINT('Ctrl Pts',(-2.30310126851141,1.05660076494221,-3.22240232769833));
#16159=CARTESIAN_POINT('Ctrl Pts',(-2.37444222349998,0.135962285121762,
-3.16041923872999));
#16160=CARTESIAN_POINT('Ctrl Pts',(-2.37324810841896,0.00196432295147262,
-3.15141010809498));
#16161=CARTESIAN_POINT('Origin',(0.,0.,-9.84858989190502));
#16162=CARTESIAN_POINT('',(-2.36970398032994,0.00191691978235058,-5.34858989190502));
#16163=CARTESIAN_POINT('',(-2.36830943662642,-0.00106730930303889,-5.15141010809498));
#16164=CARTESIAN_POINT('',(-2.37175,-6.37235396393925E-14,-9.84858989190502));
#16165=CARTESIAN_POINT('Ctrl Pts',(-2.36970398032994,0.00191691978235074,
-5.34858989190502));
#16166=CARTESIAN_POINT('Ctrl Pts',(-2.36566369524077,-0.533511972470332,
-5.31272819550281));
#16167=CARTESIAN_POINT('Ctrl Pts',(-1.920436581503,-1.8670796650718,-5.22381660582723));
#16168=CARTESIAN_POINT('Ctrl Pts',(0.294454856588238,-2.79006777499793,
-5.08185512287827));
#16169=CARTESIAN_POINT('Ctrl Pts',(2.50681415110888,-1.25978745570213,-4.92270544305818));
#16170=CARTESIAN_POINT('Ctrl Pts',(2.41455925517875,1.42866531011816,-4.76355576323806));
#16171=CARTESIAN_POINT('Ctrl Pts',(0.102504271982408,2.80368940376361,-4.60440608341796));
#16172=CARTESIAN_POINT('Ctrl Pts',(-1.98887866909948,1.75854255405241,-4.46608412630694));
#16173=CARTESIAN_POINT('Ctrl Pts',(-2.36612921203186,0.480355695668269,
-4.38081206246929));
#16174=CARTESIAN_POINT('Ctrl Pts',(-2.36855400559966,-0.00132034435408088,
-4.34858989190502));
#16175=CARTESIAN_POINT('Ctrl Pts',(-2.36830943662642,-0.00106730930303865,
-5.15141010809498));
#16176=CARTESIAN_POINT('Ctrl Pts',(-2.36964081130378,-0.329574131799768,
-5.12944007206332));
#16177=CARTESIAN_POINT('Ctrl Pts',(-2.15248665188282,-1.44849051785314,
-5.05449607769833));
#16178=CARTESIAN_POINT('Ctrl Pts',(-0.441597707549828,-2.76921495982712,
-4.926578125));
#16179=CARTESIAN_POINT('Ctrl Pts',(2.0888801521554,-1.870865869044,-4.76765625));
#16180=CARTESIAN_POINT('Ctrl Pts',(2.70399705609256,0.742939933921091,-4.608734375));
#16181=CARTESIAN_POINT('Ctrl Pts',(0.839732362462355,2.67552038173531,-4.4498125));
#16182=CARTESIAN_POINT('Ctrl Pts',(-1.68709171325523,2.17606294290117,-4.29737107769833));
#16183=CARTESIAN_POINT('Ctrl Pts',(-2.36896312957456,0.689158080288809,
-4.19790361372999));
#16184=CARTESIAN_POINT('Ctrl Pts',(-2.37427834230277,-0.00158579729887398,
-4.15141010809498));
#16185=CARTESIAN_POINT('Origin',(0.,0.,-9.84858989190502));
#16186=CARTESIAN_POINT('',(-2.37551517139031,0.000588138520267321,-6.34858989190503));
#16187=CARTESIAN_POINT('',(-2.37036013955411,0.00206597193358679,-6.15141010809498));
#16188=CARTESIAN_POINT('',(-2.37175,-6.37235396393925E-14,-9.84858989190502));
#16189=CARTESIAN_POINT('Ctrl Pts',(-2.37551517139031,0.000588138520267192,
-6.34858989190502));
#16190=CARTESIAN_POINT('Ctrl Pts',(-2.37299028602682,-0.75453010380037,
-6.2976942218097));
#16191=CARTESIAN_POINT('Ctrl Pts',(-1.57431214687729,-2.30130303879988,
-6.19374865844099));
#16192=CARTESIAN_POINT('Ctrl Pts',(1.06282132621106,-2.59645975535387,-6.03675320179892));
#16193=CARTESIAN_POINT('Ctrl Pts',(2.75907820786381,-0.508617350322671,
-5.87760352197883));
#16194=CARTESIAN_POINT('Ctrl Pts',(1.91878831253368,2.04680647949509,-5.7184538421587));
#16195=CARTESIAN_POINT('Ctrl Pts',(-0.685511273604884,2.72052538198363,
-5.55930416233861));
#16196=CARTESIAN_POINT('Ctrl Pts',(-2.21477055637751,1.30492154112468,-5.4360161789207));
#16197=CARTESIAN_POINT('Ctrl Pts',(-2.37164045357285,0.258543296497135,
-5.36577808877617));
#16198=CARTESIAN_POINT('Ctrl Pts',(-2.36970398032994,0.00191691978235074,
-5.34858989190502));
#16199=CARTESIAN_POINT('Ctrl Pts',(-2.37036013955411,0.00206597193358676,
-6.15141010809498));
#16200=CARTESIAN_POINT('Ctrl Pts',(-2.36570275369349,-0.5568269279803,-6.11395048872999));
#16201=CARTESIAN_POINT('Ctrl Pts',(-1.88889845039965,-1.9132307197956,-6.02351691103166));
#16202=CARTESIAN_POINT('Ctrl Pts',(0.374189682251391,-2.77913011091259,
-5.88010937499999));
#16203=CARTESIAN_POINT('Ctrl Pts',(2.53898480026785,-1.19042008723587,-5.7211875));
#16204=CARTESIAN_POINT('Ctrl Pts',(2.37571150505774,1.48981793161623,-5.562265625));
#16205=CARTESIAN_POINT('Ctrl Pts',(0.0340680162793398,2.80399746681091,
-5.40334375));
#16206=CARTESIAN_POINT('Ctrl Pts',(-2.01077439008208,1.72085901427313,-5.26639191103166));
#16207=CARTESIAN_POINT('Ctrl Pts',(-2.36643061234994,0.462518639558447,
-5.18241403039665));
#16208=CARTESIAN_POINT('Ctrl Pts',(-2.36830943662642,-0.00106730930303865,
-5.15141010809498));
#16209=CARTESIAN_POINT('Origin',(0.,0.,-9.84858989190502));
#16210=CARTESIAN_POINT('',(-2.37144645257593,-0.00213225654898071,-7.34858989190502));
#16211=CARTESIAN_POINT('',(-2.37545655236239,-0.000153013793341117,-7.15141010809498));
#16212=CARTESIAN_POINT('',(-2.37175,-6.37235396393925E-14,-9.84858989190502));
#16213=CARTESIAN_POINT('Ctrl Pts',(-2.37144645257593,-0.00213225654898062,
-7.34858989190502));
#16214=CARTESIAN_POINT('Ctrl Pts',(-2.37340091284414,-0.194187485402639,
-7.33571014138994));
#16215=CARTESIAN_POINT('Ctrl Pts',(-2.26509829059805,-1.17526209296292,
-7.26978049760149));
#16216=CARTESIAN_POINT('Ctrl Pts',(-0.903098151772226,-2.65539425532298,
-7.15080096053969));
#16217=CARTESIAN_POINT('Ctrl Pts',(1.74597935598366,-2.19600765141715,-6.99165128071957));
#16218=CARTESIAN_POINT('Ctrl Pts',(2.79147243493216,0.283269578050224,-6.83250160089946));
#16219=CARTESIAN_POINT('Ctrl Pts',(1.26983859810019,2.50159785776548,-6.67335192107936));
#16220=CARTESIAN_POINT('Ctrl Pts',(-1.4187825692111,2.42038344679719,-6.51420224125925));
#16221=CARTESIAN_POINT('Ctrl Pts',(-2.36052316049386,0.85148752188555,-6.40594823153447));
#16222=CARTESIAN_POINT('Ctrl Pts',(-2.37562204033538,0.0325494667967356,
-6.35074411508306));
#16223=CARTESIAN_POINT('Ctrl Pts',(-2.37551517139031,0.000588138520267192,
-6.34858989190502));
#16224=CARTESIAN_POINT('Ctrl Pts',(-2.37545655236239,-0.000153013793341093,
-7.15141010809498));
#16225=CARTESIAN_POINT('Ctrl Pts',(-2.37523396052925,-0.785743332277421,
-7.09846090539666));
#16226=CARTESIAN_POINT('Ctrl Pts',(-1.51966847852805,-2.3564332885926,-6.99253774436499));
#16227=CARTESIAN_POINT('Ctrl Pts',(1.15851212495977,-2.55397203032575,-6.833640625));
#16228=CARTESIAN_POINT('Ctrl Pts',(2.77407199314419,-0.40912796830676,-6.67471874999999));
#16229=CARTESIAN_POINT('Ctrl Pts',(1.8463937974617,2.11054799657883,-6.515796875));
#16230=CARTESIAN_POINT('Ctrl Pts',(-0.774509592452447,2.6951571659338,-6.356875));
#16231=CARTESIAN_POINT('Ctrl Pts',(-2.23477737601306,1.2531335513165,-6.23541274436499));
#16232=CARTESIAN_POINT('Ctrl Pts',(-2.37228905031649,0.233537995495179,
-6.16692444706332));
#16233=CARTESIAN_POINT('Ctrl Pts',(-2.37036013955411,0.00206597193358676,
-6.15141010809498));
#16234=CARTESIAN_POINT('Origin',(0.,0.,-8.));
#16235=CARTESIAN_POINT('',(-2.94667044765691,0.000729547181041925,-6.67782388291041));
#16236=CARTESIAN_POINT('',(-2.94659773460531,-0.000189803554299958,-6.8221761170896));
#16237=CARTESIAN_POINT('',(-2.942,-3.60291088309151E-16,-8.));
#16238=CARTESIAN_POINT('',(2.14313711407335,2.01103068470337,-7.058));
#16239=CARTESIAN_POINT('Ctrl Pts',(-2.94667044765691,0.000729547181041925,
-6.67782388291041));
#16240=CARTESIAN_POINT('Ctrl Pts',(-2.94680301155969,0.0403754743611319,
-6.67997810608845));
#16241=CARTESIAN_POINT('Ctrl Pts',(-2.94607214562671,0.0800164233561188,
-6.68213232926648));
#16242=CARTESIAN_POINT('Ctrl Pts',(-2.94446266714682,0.119621710015898,
-6.68428655244452));
#16243=CARTESIAN_POINT('Ctrl Pts',(-2.90482765511341,1.09494137595425,-6.73733644571789));
#16244=CARTESIAN_POINT('Ctrl Pts',(-2.33236709384089,2.04863398522122,-6.79038633899126));
#16245=CARTESIAN_POINT('Ctrl Pts',(-1.49029383690514,2.54227047973339,-6.84343623226463));
#16246=CARTESIAN_POINT('Ctrl Pts',(-0.648220579969394,3.03590697424557,
-6.896486125538));
#16247=CARTESIAN_POINT('Ctrl Pts',(0.463465372629582,3.06948735400294,-6.94953601881137));
#16248=CARTESIAN_POINT('Ctrl Pts',(1.33388947734758,2.62766247069921,-7.00258591208474));
#16249=CARTESIAN_POINT('Ctrl Pts',(1.63696113867246,2.47382412836503,-7.02105727472316));
#16250=CARTESIAN_POINT('Ctrl Pts',(1.91078336440736,2.26234991967576,-7.03952863736158));
#16251=CARTESIAN_POINT('Ctrl Pts',(2.14313711407335,2.01103068470337,-7.058));
#16252=CARTESIAN_POINT('',(-0.260781672665176,2.92495925220595,-7.058));
#16253=CARTESIAN_POINT('Origin',(0.,0.,-7.058));
#16254=CARTESIAN_POINT('Ctrl Pts',(-0.260780188608352,2.92495057073752,
-7.058));
#16255=CARTESIAN_POINT('Ctrl Pts',(-0.734528747633871,2.88336670063893,
-7.03239075299821));
#16256=CARTESIAN_POINT('Ctrl Pts',(-1.19860833266692,2.73328273370447,-7.00678150599641));
#16257=CARTESIAN_POINT('Ctrl Pts',(-1.59511647381414,2.47846404445,-6.98117225899462));
#16258=CARTESIAN_POINT('Ctrl Pts',(-2.41569591362769,1.95111301282311,-6.92817354502628));
#16259=CARTESIAN_POINT('Ctrl Pts',(-2.94687410332821,0.975194558044649,
-6.87517483105794));
#16260=CARTESIAN_POINT('Ctrl Pts',(-2.94659773460531,-0.000189803554299958,
-6.8221761170896));
#16261=CARTESIAN_POINT('Origin',(0.,0.,-8.));
#16262=CARTESIAN_POINT('',(-2.9394620470668,0.00237781300715098,-5.67782388291041));
#16263=CARTESIAN_POINT('',(-2.9402759694606,0.00256270240486823,-5.8221761170896));
#16264=CARTESIAN_POINT('',(-2.942,-3.60291088309151E-16,-8.));
#16265=CARTESIAN_POINT('Ctrl Pts',(-2.9394620470668,0.00237781300715098,
-5.67782388291041));
#16266=CARTESIAN_POINT('Ctrl Pts',(-2.94186411485667,0.32070596744792,-5.69501207978156));
#16267=CARTESIAN_POINT('Ctrl Pts',(-2.89424613177562,0.638334922651543,
-5.71220027665272));
#16268=CARTESIAN_POINT('Ctrl Pts',(-2.79356335203011,0.938143544427409,
-5.72938847352388));
#16269=CARTESIAN_POINT('Ctrl Pts',(-2.48281460043022,1.86347710366387,-5.78243836679725));
#16270=CARTESIAN_POINT('Ctrl Pts',(-1.66657314124927,2.61905502148427,-5.83548826007062));
#16271=CARTESIAN_POINT('Ctrl Pts',(-0.720041998643112,2.85755997694263,
-5.88853815334399));
#16272=CARTESIAN_POINT('Ctrl Pts',(0.226489143963049,3.096064932401,-5.94158804661735));
#16273=CARTESIAN_POINT('Ctrl Pts',(1.30330996999442,2.81749692549733,-5.99463793989072));
#16274=CARTESIAN_POINT('Ctrl Pts',(2.01544111468229,2.14990703628435,-6.04768783316409));
#16275=CARTESIAN_POINT('Ctrl Pts',(2.72757225937017,1.48231714707138,-6.10073772643746));
#16276=CARTESIAN_POINT('Ctrl Pts',(3.07501372271456,0.425705375549109,-6.15378761971083));
#16277=CARTESIAN_POINT('Ctrl Pts',(2.89805192420001,-0.534239058091705,
-6.2068375129842));
#16278=CARTESIAN_POINT('Ctrl Pts',(2.72109012568547,-1.49418349173252,-6.25988740625757));
#16279=CARTESIAN_POINT('Ctrl Pts',(2.01972506531199,-2.35746058749187,-6.31293729953094));
#16280=CARTESIAN_POINT('Ctrl Pts',(1.11636310017402,-2.72724142168666,-6.36598719280431));
#16281=CARTESIAN_POINT('Ctrl Pts',(0.213001135036057,-3.09702225588146,
-6.41903708607767));
#16282=CARTESIAN_POINT('Ctrl Pts',(-0.892357734866394,-2.97330682851169,
-6.47208697935105));
#16283=CARTESIAN_POINT('Ctrl Pts',(-1.69163243842047,-2.41297575352194,
-6.52513687262442));
#16284=CARTESIAN_POINT('Ctrl Pts',(-2.45845059991998,-1.87539831882508,
-6.57603254271975));
#16285=CARTESIAN_POINT('Ctrl Pts',(-2.94353849330279,-0.935945004903834,
-6.62692821281508));
#16286=CARTESIAN_POINT('Ctrl Pts',(-2.94667044765691,0.000729547181041925,
-6.67782388291041));
#16287=CARTESIAN_POINT('Ctrl Pts',(-2.94659773460531,-0.000189803554299958,
-6.8221761170896));
#16288=CARTESIAN_POINT('Ctrl Pts',(-2.94632162406539,-0.97466296344897,
-6.76922691439127));
#16289=CARTESIAN_POINT('Ctrl Pts',(-2.41580926507918,-1.94860411873223,
-6.71627771169294));
#16290=CARTESIAN_POINT('Ctrl Pts',(-1.59710847501959,-2.47650521211642,
-6.66332850899462));
#16291=CARTESIAN_POINT('Ctrl Pts',(-0.778024913229645,-3.00465311803264,
-6.61035455066128));
#16292=CARTESIAN_POINT('Ctrl Pts',(0.329516619306248,-3.08634378537204,
-6.55738059232795));
#16293=CARTESIAN_POINT('Ctrl Pts',(1.217286692148,-2.68376610295237,-6.50440663399462));
#16294=CARTESIAN_POINT('Ctrl Pts',(2.10505676498976,-2.2811884205327,-6.45143267566128));
#16295=CARTESIAN_POINT('Ctrl Pts',(2.77305537813738,-1.39434238835395,-6.39845871732794));
#16296=CARTESIAN_POINT('Ctrl Pts',(2.91526737915637,-0.43000396601087,-6.34548475899461));
#16297=CARTESIAN_POINT('Ctrl Pts',(3.05747938017536,0.534334456332214,-6.29251080066128));
#16298=CARTESIAN_POINT('Ctrl Pts',(2.67390476906572,1.57616526883964,-6.23953684232795));
#16299=CARTESIAN_POINT('Ctrl Pts',(1.94027439593581,2.21794221729091,-6.18656288399462));
#16300=CARTESIAN_POINT('Ctrl Pts',(1.20664402280589,2.85971916574218,-6.13358892566128));
#16301=CARTESIAN_POINT('Ctrl Pts',(0.122957887655704,3.1014422501373,-6.08061496732794));
#16302=CARTESIAN_POINT('Ctrl Pts',(-0.813885412179048,2.8322385802483,-6.02764100899461));
#16303=CARTESIAN_POINT('Ctrl Pts',(-1.7507287120138,2.5630349103593,-5.97466705066128));
#16304=CARTESIAN_POINT('Ctrl Pts',(-2.54072917653311,1.78290448618619,-5.92169309232795));
#16305=CARTESIAN_POINT('Ctrl Pts',(-2.82173256992598,0.849537273856912,
-5.86871913399462));
#16306=CARTESIAN_POINT('Ctrl Pts',(-2.90402926878541,0.576184559247742,
-5.85320479502628));
#16307=CARTESIAN_POINT('Ctrl Pts',(-2.9426686564904,0.289688534941257,-5.83769045605794));
#16308=CARTESIAN_POINT('Ctrl Pts',(-2.9402759694606,0.00256270240486823,
-5.8221761170896));
#16309=CARTESIAN_POINT('Origin',(0.,0.,-8.));
#16310=CARTESIAN_POINT('',(-2.93803557899197,-0.00163780039619282,-4.6778238829104));
#16311=CARTESIAN_POINT('',(-2.9377322072541,-0.00132392704517904,-4.8221761170896));
#16312=CARTESIAN_POINT('',(-2.942,-3.60291088309151E-16,-8.));
#16313=CARTESIAN_POINT('Ctrl Pts',(-2.93803557899197,-0.00163780039619282,
-4.6778238829104));
#16314=CARTESIAN_POINT('Ctrl Pts',(-2.93502778193221,0.595849670773092,
-4.71004605347468));
#16315=CARTESIAN_POINT('Ctrl Pts',(-2.75819953128571,1.19497285403097,-4.74226822403896));
#16316=CARTESIAN_POINT('Ctrl Pts',(-2.41983077500895,1.68182270057143,-4.77449039460323));
#16317=CARTESIAN_POINT('Ctrl Pts',(-1.86274768305156,2.48336188762304,-4.8275402878766));
#16318=CARTESIAN_POINT('Ctrl Pts',(-0.867798935196638,2.98057716514018,
-4.88059018114997));
#16319=CARTESIAN_POINT('Ctrl Pts',(0.107667481214478,2.94491363398168,-4.93364007442334));
#16320=CARTESIAN_POINT('Ctrl Pts',(1.08313389762559,2.90925010282318,-4.98668996769671));
#16321=CARTESIAN_POINT('Ctrl Pts',(2.0391179825929,2.34070776298903,-5.03973986097007));
#16322=CARTESIAN_POINT('Ctrl Pts',(2.53618271428821,1.50062843193614,-5.09278975424345));
#16323=CARTESIAN_POINT('Ctrl Pts',(3.0332474459835,0.660549100883245,-5.14583964751682));
#16324=CARTESIAN_POINT('Ctrl Pts',(3.0713928244068,-0.451067221388398,-5.19888954079019));
#16325=CARTESIAN_POINT('Ctrl Pts',(2.63308446274324,-1.32324407648214,-5.25193943406356));
#16326=CARTESIAN_POINT('Ctrl Pts',(2.19477610107968,-2.19542093157588,-5.30498932733693));
#16327=CARTESIAN_POINT('Ctrl Pts',(1.28001399932924,-2.82815831949173,-5.35803922061029));
#16328=CARTESIAN_POINT('Ctrl Pts',(0.309286933579615,-2.93060579823407,
-5.41108911388366));
#16329=CARTESIAN_POINT('Ctrl Pts',(-0.661440132170006,-3.03305327697642,
-5.46413900715703));
#16330=CARTESIAN_POINT('Ctrl Pts',(-1.68813216191882,-2.60521084654528,
-5.5171889004304));
#16331=CARTESIAN_POINT('Ctrl Pts',(-2.29885015478382,-1.84374503100344,
-5.57023879370377));
#16332=CARTESIAN_POINT('Ctrl Pts',(-2.71169515589689,-1.32899459113155,
-5.60610049010599));
#16333=CARTESIAN_POINT('Ctrl Pts',(-2.93445033894734,-0.661786538635051,
-5.6419621865082));
#16334=CARTESIAN_POINT('Ctrl Pts',(-2.9394620470668,0.00237781300715098,
-5.67782388291041));
#16335=CARTESIAN_POINT('Ctrl Pts',(-2.9402759694606,0.00256270240486823,
-5.8221761170896));
#16336=CARTESIAN_POINT('Ctrl Pts',(-2.93449878839097,-0.690707208650971,
-5.7847164977246));
#16337=CARTESIAN_POINT('Ctrl Pts',(-2.68950923101698,-1.38764883078321,
-5.74725687835961));
#16338=CARTESIAN_POINT('Ctrl Pts',(-2.24226106065643,-1.9121176582849,-5.70979725899461));
#16339=CARTESIAN_POINT('Ctrl Pts',(-1.60977983572761,-2.65380137761201,
-5.65682330066128));
#16340=CARTESIAN_POINT('Ctrl Pts',(-0.572811063603553,-3.05056481578078,
-5.60384934232795));
#16341=CARTESIAN_POINT('Ctrl Pts',(0.393221000839735,-2.92049813954126,
-5.55087538399462));
#16342=CARTESIAN_POINT('Ctrl Pts',(1.35925306528302,-2.79043146330174,-5.49790142566129));
#16343=CARTESIAN_POINT('Ctrl Pts',(2.25434842204554,-2.13353467265391,-5.44492746732795));
#16344=CARTESIAN_POINT('Ctrl Pts',(2.66814113507013,-1.25097642514893,-5.39195350899461));
#16345=CARTESIAN_POINT('Ctrl Pts',(3.08193384809471,-0.368418177643935,
-5.33897955066128));
#16346=CARTESIAN_POINT('Ctrl Pts',(3.01442391738137,0.739801526718225,-5.28600559232795));
#16347=CARTESIAN_POINT('Ctrl Pts',(2.49655981011218,1.56560360282277,-5.23303163399462));
#16348=CARTESIAN_POINT('Ctrl Pts',(1.978695702843,2.39140567892731,-5.18005767566128));
#16349=CARTESIAN_POINT('Ctrl Pts',(1.01047741901797,2.93479012677422,-5.12708371732795));
#16350=CARTESIAN_POINT('Ctrl Pts',(0.0358014650438746,2.94663260578348,
-5.07410975899461));
#16351=CARTESIAN_POINT('Ctrl Pts',(-0.938874488930227,2.95847508479273,
-5.02113580066128));
#16352=CARTESIAN_POINT('Ctrl Pts',(-1.92000811305341,2.4387755949643,-4.96816184232795));
#16353=CARTESIAN_POINT('Ctrl Pts',(-2.45778367776644,1.62579923282352,-4.91518788399462));
#16354=CARTESIAN_POINT('Ctrl Pts',(-2.77252609741322,1.14999080245654,-4.88418396169294));
#16355=CARTESIAN_POINT('Ctrl Pts',(-2.93540164921829,0.573723974947211,
-4.85318003939127));
#16356=CARTESIAN_POINT('Ctrl Pts',(-2.9377322072541,-0.00132392704517904,
-4.8221761170896));
#16357=CARTESIAN_POINT('Origin',(0.,0.,-8.));
#16358=CARTESIAN_POINT('',(-2.9454696039649,-0.00181482317371945,-3.67782388291041));
#16359=CARTESIAN_POINT('',(-2.9451362424601,-0.0019670773281975,-3.8221761170896));
#16360=CARTESIAN_POINT('',(-2.942,-3.60291088309151E-16,-8.));
#16361=CARTESIAN_POINT('Ctrl Pts',(-2.9454696039649,-0.00181482317371945,
-3.67782388291041));
#16362=CARTESIAN_POINT('Ctrl Pts',(-2.93917517943113,0.868803733747646,
-3.7250800271678));
#16363=CARTESIAN_POINT('Ctrl Pts',(-2.5291560477708,1.74457197301595,-3.77233617142519));
#16364=CARTESIAN_POINT('Ctrl Pts',(-1.85306766288973,2.2913421391832,-3.81959231568259));
#16365=CARTESIAN_POINT('Ctrl Pts',(-1.09408875707911,2.90514801387,-3.87264220895595));
#16366=CARTESIAN_POINT('Ctrl Pts',(0.00020064814866938,3.10433811892754,
-3.92569210222932));
#16367=CARTESIAN_POINT('Ctrl Pts',(0.926788687436315,2.79735076364636,-3.97874199550269));
#16368=CARTESIAN_POINT('Ctrl Pts',(1.85337672672397,2.49036340836518,-4.03179188877606));
#16369=CARTESIAN_POINT('Ctrl Pts',(2.61226340007148,1.67719859274527,-4.08484178204943));
#16370=CARTESIAN_POINT('Ctrl Pts',(2.85461137223702,0.731643680721236,-4.1378916753228));
#16371=CARTESIAN_POINT('Ctrl Pts',(3.09695934440256,-0.213911231302795,
-4.19094156859617));
#16372=CARTESIAN_POINT('Ctrl Pts',(2.82276861538611,-1.29185623973094,-4.24399146186954));
#16373=CARTESIAN_POINT('Ctrl Pts',(2.1580763990752,-2.00669250775953,-4.29704135514291));
#16374=CARTESIAN_POINT('Ctrl Pts',(1.49338418276429,-2.72152877578811,-4.35009124841628));
#16375=CARTESIAN_POINT('Ctrl Pts',(0.438190479158908,-3.07325630341714,
-4.40314114168965));
#16376=CARTESIAN_POINT('Ctrl Pts',(-0.522463958417041,-2.90019654199934,
-4.45619103496301));
#16377=CARTESIAN_POINT('Ctrl Pts',(-1.483118395993,-2.72713678058155,-4.50924092823638));
#16378=CARTESIAN_POINT('Ctrl Pts',(-2.34923356753954,-2.02928973011691,
-4.56229082150976));
#16379=CARTESIAN_POINT('Ctrl Pts',(-2.72268243528287,-1.12743465659155,
-4.61534071478313));
#16380=CARTESIAN_POINT('Ctrl Pts',(-2.8693008162719,-0.773360666312599,
-4.63616843749222));
#16381=CARTESIAN_POINT('Ctrl Pts',(-2.93997975475756,-0.387840937979601,
-4.65699616020131));
#16382=CARTESIAN_POINT('Ctrl Pts',(-2.93803557899197,-0.00163780039619282,
-4.6778238829104));
#16383=CARTESIAN_POINT('Ctrl Pts',(-2.9377322072541,-0.00132392704517904,
-4.8221761170896));
#16384=CARTESIAN_POINT('Ctrl Pts',(-2.93938369004142,-0.408815050386763,
-4.80020608105794));
#16385=CARTESIAN_POINT('Ctrl Pts',(-2.86041847102297,-0.815694097620487,
-4.77823604502627));
#16386=CARTESIAN_POINT('Ctrl Pts',(-2.69774861387726,-1.18578124140415,
-4.75626600899461));
#16387=CARTESIAN_POINT('Ctrl Pts',(-2.30552047997214,-2.07813211903793,
-4.70329205066128));
#16388=CARTESIAN_POINT('Ctrl Pts',(-1.42664670685898,-2.75658063985234,
-4.65031809232795));
#16389=CARTESIAN_POINT('Ctrl Pts',(-0.464061240614209,-2.91008106588381,
-4.59734413399462));
#16390=CARTESIAN_POINT('Ctrl Pts',(0.498524225630561,-3.06358149191529,
-4.54437017566128));
#16391=CARTESIAN_POINT('Ctrl Pts',(1.54482138500695,-2.69213382316382,-4.49139621732795));
#16392=CARTESIAN_POINT('Ctrl Pts',(2.19513864684848,-1.96603426957068,-4.43842225899462));
#16393=CARTESIAN_POINT('Ctrl Pts',(2.84545590869002,-1.23993471597753,-4.38544830066128));
#16394=CARTESIAN_POINT('Ctrl Pts',(3.0997932729967,-0.159183277542723,-4.33247434232795));
#16395=CARTESIAN_POINT('Ctrl Pts',(2.84154565012492,0.780732280574893,-4.27950038399461));
#16396=CARTESIAN_POINT('Ctrl Pts',(2.58329802725314,1.72064783869251,-4.22652642566128));
#16397=CARTESIAN_POINT('Ctrl Pts',(1.81246541720289,2.51972751649293,-4.17355246732795));
#16398=CARTESIAN_POINT('Ctrl Pts',(0.882448402231475,2.81162041693353,-4.12057850899462));
#16399=CARTESIAN_POINT('Ctrl Pts',(-0.0475686127399455,3.10351331737414,
-4.06760455066128));
#16400=CARTESIAN_POINT('Ctrl Pts',(-1.13677003263254,2.88821944045492,-4.01463059232795));
#16401=CARTESIAN_POINT('Ctrl Pts',(-1.885794036659,2.26444372326888,-3.96165663399461));
#16402=CARTESIAN_POINT('Ctrl Pts',(-2.54318783632236,1.71697623670729,-3.91516312835961));
#16403=CARTESIAN_POINT('Ctrl Pts',(-2.93854307039457,0.85485530608613,-3.8686696227246));
#16404=CARTESIAN_POINT('Ctrl Pts',(-2.9451362424601,-0.0019670773281975,
-3.8221761170896));
#16405=CARTESIAN_POINT('Origin',(0.,0.,-8.));
#16406=CARTESIAN_POINT('',(-2.94375189758287,0.002485178828774,-2.6778238829104));
#16407=CARTESIAN_POINT('',(-2.94385830503576,0.00243661352308097,-2.8221761170896));
#16408=CARTESIAN_POINT('',(-2.942,-3.60291088309151E-16,-8.));
#16409=CARTESIAN_POINT('Ctrl Pts',(-2.94375189758287,0.002485178828774,
-2.6778238829104));
#16410=CARTESIAN_POINT('Ctrl Pts',(-2.94528921136235,0.172980281625067,
-2.68706410758755));
#16411=CARTESIAN_POINT('Ctrl Pts',(-2.93175845086741,0.343231533938287,
-2.69630433226469));
#16412=CARTESIAN_POINT('Ctrl Pts',(-2.90229484040136,0.510679286112688,
-2.70554455694183));
#16413=CARTESIAN_POINT('Ctrl Pts',(-2.73313862988857,1.47202878702813,-2.7585944502152));
#16414=CARTESIAN_POINT('Ctrl Pts',(-2.03881541363051,2.34097135659234,-2.81164434348857));
#16415=CARTESIAN_POINT('Ctrl Pts',(-1.13848469599121,2.7180803976305,-2.86469423676194));
#16416=CARTESIAN_POINT('Ctrl Pts',(-0.238153978351924,3.09518943866866,
-2.91774413003531));
#16417=CARTESIAN_POINT('Ctrl Pts',(0.868184240668593,2.98046495118077,-2.97079402330868));
#16418=CARTESIAN_POINT('Ctrl Pts',(1.67197964215867,2.42664226336089,-3.02384391658205));
#16419=CARTESIAN_POINT('Ctrl Pts',(2.47577504364874,1.87281957554101,-3.07689380985541));
#16420=CARTESIAN_POINT('Ctrl Pts',(2.97702762760836,0.879898687389133,-3.12994370312878));
#16421=CARTESIAN_POINT('Ctrl Pts',(2.9453266735165,-0.0957045563702386,
-3.18299359640215));
#16422=CARTESIAN_POINT('Ctrl Pts',(2.91362571942463,-1.07130780012962,-3.23604348967552));
#16423=CARTESIAN_POINT('Ctrl Pts',(2.34897122728125,-2.02959339949651,-3.28909338294889));
#16424=CARTESIAN_POINT('Ctrl Pts',(1.51091785855076,-2.53006635742898,-3.34214327622226));
#16425=CARTESIAN_POINT('Ctrl Pts',(0.672864489820277,-3.03053931536144,
-3.39519316949563));
#16426=CARTESIAN_POINT('Ctrl Pts',(-0.438587755497323,-3.0731996318595,
-3.448243062769));
#16427=CARTESIAN_POINT('Ctrl Pts',(-1.31253777493485,-2.63843763607156,
-3.50129295604237));
#16428=CARTESIAN_POINT('Ctrl Pts',(-2.18648779437236,-2.20367564028361,
-3.55434284931574));
#16429=CARTESIAN_POINT('Ctrl Pts',(-2.8229355879298,-1.29149133220967,-3.60739274258911));
#16430=CARTESIAN_POINT('Ctrl Pts',(-2.9293252815118,-0.321188356014672,
-3.66044263586248));
#16431=CARTESIAN_POINT('Ctrl Pts',(-2.94094444122103,-0.215218455480482,
-3.66623638487846));
#16432=CARTESIAN_POINT('Ctrl Pts',(-2.94624131982369,-0.108555343093822,
-3.67203013389443));
#16433=CARTESIAN_POINT('Ctrl Pts',(-2.9454696039649,-0.00181482317371945,
-3.67782388291041));
#16434=CARTESIAN_POINT('Ctrl Pts',(-2.9451362424601,-0.0019670773281975,
-3.8221761170896));
#16435=CARTESIAN_POINT('Ctrl Pts',(-2.94605522542598,-0.121394443596838,
-3.81569566439127));
#16436=CARTESIAN_POINT('Ctrl Pts',(-2.93942137368933,-0.240718870162436,
-3.80921521169294));
#16437=CARTESIAN_POINT('Ctrl Pts',(-2.92489152753265,-0.359073945995959,
-3.80273475899462));
#16438=CARTESIAN_POINT('Ctrl Pts',(-2.80611842621951,-1.3265583406219,-3.74976080066128));
#16439=CARTESIAN_POINT('Ctrl Pts',(-2.15972563543289,-2.22926957242092,
-3.69678684232795));
#16440=CARTESIAN_POINT('Ctrl Pts',(-1.28206228631137,-2.65334521622321,
-3.64381288399462));
#16441=CARTESIAN_POINT('Ctrl Pts',(-0.404398937189858,-3.07742086002551,
-3.59083892566128));
#16442=CARTESIAN_POINT('Ctrl Pts',(0.704534970266555,-3.02286091583108,
-3.53786496732795));
#16443=CARTESIAN_POINT('Ctrl Pts',(1.53633092845112,-2.51467926673377,-3.48489100899462));
#16444=CARTESIAN_POINT('Ctrl Pts',(2.36812688663568,-2.00649761763647,-3.43191705066128));
#16445=CARTESIAN_POINT('Ctrl Pts',(2.9227848955484,-1.04469426363629,-3.37894309232795));
#16446=CARTESIAN_POINT('Ctrl Pts',(2.94601310641574,-0.0702233526915731,
-3.32596913399462));
#16447=CARTESIAN_POINT('Ctrl Pts',(2.96924131728308,0.904247558253159,-3.27299517566128));
#16448=CARTESIAN_POINT('Ctrl Pts',(2.46103973010502,1.89138602614242,-3.22002121732795));
#16449=CARTESIAN_POINT('Ctrl Pts',(1.65440150303174,2.43862260575344,-3.16704725899461));
#16450=CARTESIAN_POINT('Ctrl Pts',(0.847763275958474,2.98585918536446,-3.11407330066128));
#16451=CARTESIAN_POINT('Ctrl Pts',(-0.257311591010001,3.09319387669725,
-3.06109934232795));
#16452=CARTESIAN_POINT('Ctrl Pts',(-1.1541838289695,2.71141738090907,-3.00812538399462));
#16453=CARTESIAN_POINT('Ctrl Pts',(-2.05105606692901,2.32964088512089,-2.95515142566128));
#16454=CARTESIAN_POINT('Ctrl Pts',(-2.73972567587954,1.45875320221174,-2.90217746732795));
#16455=CARTESIAN_POINT('Ctrl Pts',(-2.90446104077339,0.49802672031522,-2.84920350899462));
#16456=CARTESIAN_POINT('Ctrl Pts',(-2.93247711639295,0.334638696232663,
-2.84019437835961));
#16457=CARTESIAN_POINT('Ctrl Pts',(-2.94533952631471,0.168652279046411,
-2.8311852477246));
#16458=CARTESIAN_POINT('Ctrl Pts',(-2.94385830503576,0.00243661352308097,
-2.8221761170896));
#16459=CARTESIAN_POINT('Origin',(0.,0.,-8.));
#16460=CARTESIAN_POINT('',(-2.93727051546118,0.000683352736612908,-1.6778238829104));
#16461=CARTESIAN_POINT('',(-2.93727005869068,0.000602850538960121,-1.8221761170896));
#16462=CARTESIAN_POINT('',(-2.942,-3.60291088309151E-16,-8.));
#16463=CARTESIAN_POINT('Ctrl Pts',(-2.93727051546118,0.000683352736612908,
-1.6778238829104));
#16464=CARTESIAN_POINT('Ctrl Pts',(-2.93820523817054,0.451087602524798,
-1.70209808128066));
#16465=CARTESIAN_POINT('Ctrl Pts',(-2.84105703677905,0.901110116594761,
-1.72637227965093));
#16466=CARTESIAN_POINT('Ctrl Pts',(-2.64374793719726,1.30181149599908,-1.75064647802119));
#16467=CARTESIAN_POINT('Ctrl Pts',(-2.21254001366382,2.17752179084177,-1.80369637129456));
#16468=CARTESIAN_POINT('Ctrl Pts',(-1.30294720868908,2.81766625524686,-1.85674626456792));
#16469=CARTESIAN_POINT('Ctrl Pts',(-0.33308409121168,2.9279955839445,-1.90979615784129));
#16470=CARTESIAN_POINT('Ctrl Pts',(0.636779026265724,3.03832491264213,-1.96284605111466));
#16471=CARTESIAN_POINT('Ctrl Pts',(1.66691245624578,2.6188391056323,-2.01589594438803));
#16472=CARTESIAN_POINT('Ctrl Pts',(2.28379603312924,1.86236011037004,-2.0689458376614));
#16473=CARTESIAN_POINT('Ctrl Pts',(2.90067961001269,1.10588111510779,-2.12199573093477));
#16474=CARTESIAN_POINT('Ctrl Pts',(3.10431333379955,0.0124089315930999,
-2.17504562420814));
#16475=CARTESIAN_POINT('Ctrl Pts',(2.80109232700541,-0.915418640485284,
-2.22809551748151));
#16476=CARTESIAN_POINT('Ctrl Pts',(2.49787132021127,-1.84324621256366,-2.28114541075488));
#16477=CARTESIAN_POINT('Ctrl Pts',(1.68779558283615,-2.60542917320574,-2.33419530402825));
#16478=CARTESIAN_POINT('Ctrl Pts',(0.743232829830214,-2.85161581110816,
-2.38724519730162));
#16479=CARTESIAN_POINT('Ctrl Pts',(-0.201329923175726,-3.09780244901058,
-2.44029509057498));
#16480=CARTESIAN_POINT('Ctrl Pts',(-1.28037969181247,-2.82799276417333,
-2.49334498384836));
#16481=CARTESIAN_POINT('Ctrl Pts',(-1.99790997374708,-2.16620970562137,
-2.54639487712172));
#16482=CARTESIAN_POINT('Ctrl Pts',(-2.59046090871931,-1.61969594868771,
-2.59020454571795));
#16483=CARTESIAN_POINT('Ctrl Pts',(-2.93646319957384,-0.805864640766195,
-2.63401421431418));
#16484=CARTESIAN_POINT('Ctrl Pts',(-2.94375189758287,0.002485178828774,
-2.6778238829104));
#16485=CARTESIAN_POINT('Ctrl Pts',(-2.94385830503576,0.00243661352308097,
-2.8221761170896));
#16486=CARTESIAN_POINT('Ctrl Pts',(-2.93662990077009,-0.808700819327745,
-2.77821128939127));
#16487=CARTESIAN_POINT('Ctrl Pts',(-2.58781232696644,-1.62529773088275,
-2.73424646169294));
#16488=CARTESIAN_POINT('Ctrl Pts',(-1.99154488867446,-2.17202061041561,
-2.69028163399462));
#16489=CARTESIAN_POINT('Ctrl Pts',(-1.27309225084451,-2.83077617836602,
-2.63730767566128));
#16490=CARTESIAN_POINT('Ctrl Pts',(-0.195385854347449,-3.09772203338294,
-2.58433371732795));
#16491=CARTESIAN_POINT('Ctrl Pts',(0.747482555863827,-2.85047263742232,
-2.53135975899461));
#16492=CARTESIAN_POINT('Ctrl Pts',(1.6903509660751,-2.6032232414617,-2.47838580066128));
#16493=CARTESIAN_POINT('Ctrl Pts',(2.49838139000059,-1.84177859452355,-2.42541184232795));
#16494=CARTESIAN_POINT('Ctrl Pts',(2.80111931520967,-0.915235066534927,
-2.37243788399462));
#16495=CARTESIAN_POINT('Ctrl Pts',(3.10385724041874,0.0113084614536957,
-2.31946392566128));
#16496=CARTESIAN_POINT('Ctrl Pts',(2.9013026669114,1.10295087049279,-2.26648996732795));
#16497=CARTESIAN_POINT('Ctrl Pts',(2.28632002818116,1.85921097912,-2.21351600899462));
#16498=CARTESIAN_POINT('Ctrl Pts',(1.67133738945091,2.61547108774722,-2.16054205066128));
#16499=CARTESIAN_POINT('Ctrl Pts',(0.643926685497746,3.03634889596256,-2.10756809232795));
#16500=CARTESIAN_POINT('Ctrl Pts',(-0.324879278745637,2.92888668377361,
-2.05459413399462));
#16501=CARTESIAN_POINT('Ctrl Pts',(-1.29368524298901,2.82142447158467,-2.00162017566128));
#16502=CARTESIAN_POINT('Ctrl Pts',(-2.20388646752261,2.18562223899146,-1.94864621732795));
#16503=CARTESIAN_POINT('Ctrl Pts',(-2.63818645785514,1.31297283747813,-1.89567225899462));
#16504=CARTESIAN_POINT('Ctrl Pts',(-2.83903592378818,0.909401181612935,
-1.87117354502628));
#16505=CARTESIAN_POINT('Ctrl Pts',(-2.93810161469806,0.455173639139868,
-1.84667483105794));
#16506=CARTESIAN_POINT('Ctrl Pts',(-2.93727005869068,0.000602850538960121,
-1.8221761170896));
#16507=CARTESIAN_POINT('Origin',(0.,0.,-8.));
#16508=CARTESIAN_POINT('',(-2.94115781190101,-0.00289931852541142,-0.677823882910403));
#16509=CARTESIAN_POINT('',(-2.94163492837973,-0.00273205723265913,-0.822176117089598));
#16510=CARTESIAN_POINT('',(-2.942,-3.60291088309151E-16,-8.));
#16511=CARTESIAN_POINT('Ctrl Pts',(-2.94115781190101,-0.00289931852541142,
-0.677823882910403));
#16512=CARTESIAN_POINT('Ctrl Pts',(-2.93462928693851,0.724021610816987,
-0.717132054973782));
#16513=CARTESIAN_POINT('Ctrl Pts',(-2.66251292327982,1.45546978445239,-0.756440227037161));
#16514=CARTESIAN_POINT('Ctrl Pts',(-2.17433825692092,1.98917806070832,-0.79574839910054));
#16515=CARTESIAN_POINT('Ctrl Pts',(-1.51550289038833,2.70946510557116,-0.848798292373909));
#16516=CARTESIAN_POINT('Ctrl Pts',(-0.463140743616836,3.06959035999133,
-0.901848185647279));
#16517=CARTESIAN_POINT('Ctrl Pts',(0.498902376961032,2.90430157111178,-0.954898078920648));
#16518=CARTESIAN_POINT('Ctrl Pts',(1.46094549753889,2.73901278223222,-1.00794797219402));
#16519=CARTESIAN_POINT('Ctrl Pts',(2.33266959192314,2.04830995005292,-1.06099786546739));
#16520=CARTESIAN_POINT('Ctrl Pts',(2.71342505533895,1.14953876902873,-1.11404775874076));
#16521=CARTESIAN_POINT('Ctrl Pts',(3.09418051875477,0.250767588004519,-1.16709765201412));
#16522=CARTESIAN_POINT('Ctrl Pts',(2.98396735120216,-0.856071941864584,
-1.22014754528749));
#16523=CARTESIAN_POINT('Ctrl Pts',(2.43341813489043,-1.66212091392741,-1.27319743856086));
#16524=CARTESIAN_POINT('Ctrl Pts',(1.8828689185787,-2.46816988599023,-1.32624733183423));
#16525=CARTESIAN_POINT('Ctrl Pts',(0.891983653507839,-2.97342830024674,
-1.3792972251076));
#16526=CARTESIAN_POINT('Ctrl Pts',(-0.083742367919571,-2.94568489652514,
-1.43234711838097));
#16527=CARTESIAN_POINT('Ctrl Pts',(-1.05946838934697,-2.91794149280355,
-1.48539701165434));
#16528=CARTESIAN_POINT('Ctrl Pts',(-2.02003516713094,-2.35719627110387,
-1.53844690492771));
#16529=CARTESIAN_POINT('Ctrl Pts',(-2.52390703497687,-1.52118559761389,
-1.59149679820108));
#16530=CARTESIAN_POINT('Ctrl Pts',(-2.79722074485897,-1.06771082901965,
-1.62027249310419));
#16531=CARTESIAN_POINT('Ctrl Pts',(-2.93616245433829,-0.533245515985456,
-1.64904818800729));
#16532=CARTESIAN_POINT('Ctrl Pts',(-2.93727051546118,0.000683352736612908,
-1.6778238829104));
#16533=CARTESIAN_POINT('Ctrl Pts',(-2.93727005869068,0.000602850538960121,
-1.8221761170896));
#16534=CARTESIAN_POINT('Ctrl Pts',(-2.93630352793548,-0.527751997120677,
-1.7937008727246));
#16535=CARTESIAN_POINT('Ctrl Pts',(-2.80037799310706,-1.05657056282055,
-1.76522562835961));
#16536=CARTESIAN_POINT('Ctrl Pts',(-2.5324558003079,-1.50684874693044,-1.73675038399462));
#16537=CARTESIAN_POINT('Ctrl Pts',(-2.03402639629669,-2.34452435939227,
-1.68377642566128));
#16538=CARTESIAN_POINT('Ctrl Pts',(-1.07876883214279,-2.91037901388249,
-1.63080246732795));
#16539=CARTESIAN_POINT('Ctrl Pts',(-0.104635629080346,-2.94499075008032,
-1.57782850899462));
#16540=CARTESIAN_POINT('Ctrl Pts',(0.869497573982104,-2.97960248627815,
-1.52485455066128));
#16541=CARTESIAN_POINT('Ctrl Pts',(1.8625064159531,-2.48297130418358,-1.47188059232795));
#16542=CARTESIAN_POINT('Ctrl Pts',(2.4191289262232,-1.68277965785054,-1.41890663399462));
#16543=CARTESIAN_POINT('Ctrl Pts',(2.97575143649328,-0.882588011517496,
-1.36593267566128));
#16544=CARTESIAN_POINT('Ctrl Pts',(3.09598761506247,0.22116409905402,-1.31295871732795));
#16545=CARTESIAN_POINT('Ctrl Pts',(2.7247154876507,1.12243223163693,-1.25998475899462));
#16546=CARTESIAN_POINT('Ctrl Pts',(2.35344336023893,2.02370036421984,-1.20701080066128));
#16547=CARTESIAN_POINT('Ctrl Pts',(1.4906629268462,2.72248451881415,-1.15403684232795));
#16548=CARTESIAN_POINT('Ctrl Pts',(0.531925431096018,2.89843813313422,-1.10106288399462));
#16549=CARTESIAN_POINT('Ctrl Pts',(-0.426812064654162,3.0743917474543,-1.04808892566128));
#16550=CARTESIAN_POINT('Ctrl Pts',(-1.48150662276179,2.72751482150015,-0.995114967327949));
#16551=CARTESIAN_POINT('Ctrl Pts',(-2.14860846972942,2.01679609366237,-0.942141008994616));
#16552=CARTESIAN_POINT('Ctrl Pts',(-2.65218169374977,1.48029792209265,-0.902152711692943));
#16553=CARTESIAN_POINT('Ctrl Pts',(-2.93489516853091,0.736473846765843,
-0.86216441439127));
#16554=CARTESIAN_POINT('Ctrl Pts',(-2.94163492837973,-0.00273205723265913,
-0.822176117089598));
#16555=CARTESIAN_POINT('Origin',(0.,0.,-7.5));
#16556=CARTESIAN_POINT('',(-2.,-2.44929359829471E-16,-8.));
#16557=CARTESIAN_POINT('Origin',(0.,0.,-8.));
#16558=CARTESIAN_POINT('',(-2.54872116535053,-0.00229165091991151,-7.45095259589208));
#16559=CARTESIAN_POINT('',(-2.5,-3.06161699786838E-16,-7.5));
#16560=CARTESIAN_POINT('',(0.43944522199408,2.3306835819919,-7.62825));
#16561=CARTESIAN_POINT('Ctrl Pts',(0.439445221994064,2.3306835819919,-7.62825));
#16562=CARTESIAN_POINT('Ctrl Pts',(0.35950730762982,2.34930583235909,-7.62476133607378));
#16563=CARTESIAN_POINT('Ctrl Pts',(0.278764199343595,2.36340008398443,-7.62128689705201));
#16564=CARTESIAN_POINT('Ctrl Pts',(0.19754033703868,2.37315335070148,-7.61782195797437));
#16565=CARTESIAN_POINT('Ctrl Pts',(0.114158107745347,2.38316579161086,-7.61426494484472));
#16566=CARTESIAN_POINT('Ctrl Pts',(0.0302684811334496,2.38860350484577,
-7.61071794325263));
#16567=CARTESIAN_POINT('Ctrl Pts',(-0.0537928869498894,2.38961650778545,
-7.60717584146979));
#16568=CARTESIAN_POINT('Ctrl Pts',(-0.0939088819893571,2.3900999358075,
-7.60548547000916));
#16569=CARTESIAN_POINT('Ctrl Pts',(-0.134064139304447,2.38957491574745,
-7.60379621443857));
#16570=CARTESIAN_POINT('Ctrl Pts',(-0.174222567562762,2.38805369630578,
-7.60210751919786));
#16571=CARTESIAN_POINT('Ctrl Pts',(-0.198320922896885,2.38714083969668,
-7.60109416335384));
#16572=CARTESIAN_POINT('Ctrl Pts',(-0.222420421447383,2.3858692035713,-7.60008100928382));
#16573=CARTESIAN_POINT('Ctrl Pts',(-0.246513240972343,2.38424099601516,
-7.59906793693749));
#16574=CARTESIAN_POINT('Ctrl Pts',(-0.262247708409472,2.38317765103196,
-7.59840632264082));
#16575=CARTESIAN_POINT('Ctrl Pts',(-0.277979991167122,2.38196207006022,
-7.59774471512093));
#16576=CARTESIAN_POINT('Ctrl Pts',(-0.2936918680985,2.38059645837412,-7.59708375573829));
#16577=CARTESIAN_POINT('Ctrl Pts',(-0.379437414156161,2.37314380836678,
-7.59347665498045));
#16578=CARTESIAN_POINT('Ctrl Pts',(-0.464688261375226,2.36122031408759,
-7.58988407990206));
#16579=CARTESIAN_POINT('Ctrl Pts',(-0.549092376979852,2.34499084734367,
-7.58630079485361));
#16580=CARTESIAN_POINT('Ctrl Pts',(-0.634244405857918,2.32861756967879,
-7.58268575795952));
#16581=CARTESIAN_POINT('Ctrl Pts',(-0.718535581092846,2.30786151927559,
-7.57908017646459));
#16582=CARTESIAN_POINT('Ctrl Pts',(-0.801603640347307,2.28283889337961,
-7.57547867430154));
#16583=CARTESIAN_POINT('Ctrl Pts',(-0.854264768910885,2.26697575981018,
-7.57319549626497));
#16584=CARTESIAN_POINT('Ctrl Pts',(-0.906434273693594,2.24939685671676,
-7.57091395768995));
#16585=CARTESIAN_POINT('Ctrl Pts',(-0.958017010478469,2.23012130716734,
-7.56863268885273));
#16586=CARTESIAN_POINT('Ctrl Pts',(-0.972145435378402,2.22484176654604,
-7.5680078531528));
#16587=CARTESIAN_POINT('Ctrl Pts',(-0.98622277804679,2.21943748744756,-7.56738334854454));
#16588=CARTESIAN_POINT('Ctrl Pts',(-1.00024110670404,2.21391165688255,-7.56675941869597));
#16589=CARTESIAN_POINT('Ctrl Pts',(-1.08186648658626,2.18173606519387,-7.56312642419607));
#16590=CARTESIAN_POINT('Ctrl Pts',(-1.16155672144445,2.14541925679892,-7.55951003039887));
#16591=CARTESIAN_POINT('Ctrl Pts',(-1.2389527254794,2.10510908910794,-7.55590492027959));
#16592=CARTESIAN_POINT('Ctrl Pts',(-1.31591866988219,2.06502290941356,-7.55231984236159));
#16593=CARTESIAN_POINT('Ctrl Pts',(-1.390616753222,2.0209873367507,-7.54874592307184));
#16594=CARTESIAN_POINT('Ctrl Pts',(-1.4626804776292,1.97309843650394,-7.5451779335279));
#16595=CARTESIAN_POINT('Ctrl Pts',(-1.5227729444993,1.93316486139114,-7.54220265997348));
#16596=CARTESIAN_POINT('Ctrl Pts',(-1.58103363744146,1.89055092502882,-7.53923150969818));
#16597=CARTESIAN_POINT('Ctrl Pts',(-1.63723570611631,1.84528793751806,-7.53626145077414));
#16598=CARTESIAN_POINT('Ctrl Pts',(-1.66533674045373,1.82265644376269,-7.53477642131212));
#16599=CARTESIAN_POINT('Ctrl Pts',(-1.69292287318535,1.79936235037773,-7.53329166468791));
#16600=CARTESIAN_POINT('Ctrl Pts',(-1.71996402237359,1.77540760445319,-7.53180680191054));
#16601=CARTESIAN_POINT('Ctrl Pts',(-1.734592853604,1.76244846825458,-7.53100351478619));
#16602=CARTESIAN_POINT('Ctrl Pts',(-1.74906216596862,1.74929596081963,-7.53020019659465));
#16603=CARTESIAN_POINT('Ctrl Pts',(-1.76336702959904,1.73595023612016,-7.52939678733164));
#16604=CARTESIAN_POINT('Ctrl Pts',(-1.77433082190178,1.72572156442395,-7.52878102387374));
#16605=CARTESIAN_POINT('Ctrl Pts',(-1.78519228949581,1.71538465010188,-7.52816552606711));
#16606=CARTESIAN_POINT('Ctrl Pts',(-1.79594364956077,1.70494575402236,-7.52755060631426));
#16607=CARTESIAN_POINT('Ctrl Pts',(-1.79709455383888,1.7038282981764,-7.52748478080288));
#16608=CARTESIAN_POINT('Ctrl Pts',(-1.79824421789083,1.70270965364318,-7.52741896070807));
#16609=CARTESIAN_POINT('Ctrl Pts',(-1.79939263955324,1.70158982119388,-7.52735314599821));
#16610=CARTESIAN_POINT('Ctrl Pts',(-1.85981820858233,1.64266850754977,-7.52389022691203));
#16611=CARTESIAN_POINT('Ctrl Pts',(-1.91680672394307,1.58046245918003,-7.52044221587196));
#16612=CARTESIAN_POINT('Ctrl Pts',(-1.97033907896298,1.51537581293649,-7.51700450873067));
#16613=CARTESIAN_POINT('Ctrl Pts',(-2.02523133040966,1.44863575358186,-7.51347947261505));
#16614=CARTESIAN_POINT('Ctrl Pts',(-2.07649002117627,1.37886624042406,-7.50996527055285));
#16615=CARTESIAN_POINT('Ctrl Pts',(-2.12405982073786,1.30645857743699,-7.50645693852668));
#16616=CARTESIAN_POINT('Ctrl Pts',(-2.17237746941273,1.23291258704349,-7.502893451696));
#16617=CARTESIAN_POINT('Ctrl Pts',(-2.21688976450887,1.15664403526371,-7.49933602091887));
#16618=CARTESIAN_POINT('Ctrl Pts',(-2.25749682318216,1.07802895465018,-7.49577944435867));
#16619=CARTESIAN_POINT('Ctrl Pts',(-2.27284246751551,1.04831985712508,-7.49443539333109));
#16620=CARTESIAN_POINT('Ctrl Pts',(-2.28762993718892,1.0182753662529,-7.49309146429663));
#16621=CARTESIAN_POINT('Ctrl Pts',(-2.30185211585003,0.987914916938409,
-7.49174737651324));
#16622=CARTESIAN_POINT('Ctrl Pts',(-2.30818978888486,0.974385723870973,
-7.49114842545909));
#16623=CARTESIAN_POINT('Ctrl Pts',(-2.31441519544955,0.960793784042873,
-7.49054944288118));
#16624=CARTESIAN_POINT('Ctrl Pts',(-2.32052764172134,0.947140796183267,
-7.48995040393679));
#16625=CARTESIAN_POINT('Ctrl Pts',(-2.32597748838073,0.934967815519079,
-7.4894163018368));
#16626=CARTESIAN_POINT('Ctrl Pts',(-2.33133358181014,0.922755126093933,
-7.48888254203352));
#16627=CARTESIAN_POINT('Ctrl Pts',(-2.33659539015647,0.910505115445706,
-7.48834914975349));
#16628=CARTESIAN_POINT('Ctrl Pts',(-2.37190024202985,0.828311925782129,
-7.484770278347));
#16629=CARTESIAN_POINT('Ctrl Pts',(-2.40297018516154,0.744427201867178,
-7.48120732731796));
#16630=CARTESIAN_POINT('Ctrl Pts',(-2.4297508852343,0.659261131816419,-7.47765521995893));
#16631=CARTESIAN_POINT('Ctrl Pts',(-2.4567532615297,0.573390102871637,-7.47407371016681));
#16632=CARTESIAN_POINT('Ctrl Pts',(-2.47939547698255,0.486215506233761,
-7.4705032243038));
#16633=CARTESIAN_POINT('Ctrl Pts',(-2.49757659361956,0.39812982730928,-7.46693855854928));
#16634=CARTESIAN_POINT('Ctrl Pts',(-2.51554984330289,0.311051242839216,
-7.46341464805892));
#16635=CARTESIAN_POINT('Ctrl Pts',(-2.52916366178314,0.223081332246028,
-7.4598964253538));
#16636=CARTESIAN_POINT('Ctrl Pts',(-2.53827206334785,0.134586184014785,
-7.4563788630682));
#16637=CARTESIAN_POINT('Ctrl Pts',(-2.54295553089513,0.0890826835499858,
-7.45457016055402));
#16638=CARTESIAN_POINT('Ctrl Pts',(-2.54644698417321,0.043440188370138,
-7.45276163265044));
#16639=CARTESIAN_POINT('Ctrl Pts',(-2.54872116535053,-0.00229165091991107,
-7.45095259589208));
#16640=CARTESIAN_POINT('',(2.34668236863854,0.343918483395443,-7.62825));
#16641=CARTESIAN_POINT('Origin',(0.,0.,-7.62825));
#16642=CARTESIAN_POINT('Ctrl Pts',(-0.260780188608367,2.92495057073752,
-7.058));
#16643=CARTESIAN_POINT('Ctrl Pts',(-0.16290664670437,2.92113933331557,-7.07037763567872));
#16644=CARTESIAN_POINT('Ctrl Pts',(-0.0655009153188213,2.91268382038242,
-7.08279941895993));
#16645=CARTESIAN_POINT('Ctrl Pts',(0.0310593059060548,2.89959286742514,
-7.09528489244389));
#16646=CARTESIAN_POINT('Ctrl Pts',(0.129584552898908,2.88623551014979,-7.10802444858021));
#16647=CARTESIAN_POINT('Ctrl Pts',(0.227230615089889,2.86805205167427,-7.12083031352007));
#16648=CARTESIAN_POINT('Ctrl Pts',(0.323572833643809,2.84500022309371,-7.13372324739925));
#16649=CARTESIAN_POINT('Ctrl Pts',(0.413875801694046,2.82339340760767,-7.14580798256147));
#16650=CARTESIAN_POINT('Ctrl Pts',(0.503033721796121,2.79750880812771,-7.15796921289429));
#16651=CARTESIAN_POINT('Ctrl Pts',(0.590666117804777,2.76727297965209,-7.17022403407592));
#16652=CARTESIAN_POINT('Ctrl Pts',(0.619290588600912,2.75739667101947,-7.17422698032642));
#16653=CARTESIAN_POINT('Ctrl Pts',(0.647752008816874,2.74705582179321,-7.17823991228686));
#16654=CARTESIAN_POINT('Ctrl Pts',(0.67603622728258,2.73624706112264,-7.18226342576295));
#16655=CARTESIAN_POINT('Ctrl Pts',(0.697709689293547,2.72796458854652,-7.18534653964076));
#16656=CARTESIAN_POINT('Ctrl Pts',(0.719279093667969,2.7194073616259,-7.18843586672941));
#16657=CARTESIAN_POINT('Ctrl Pts',(0.740737874893652,2.71057371154558,-7.19153167510431));
#16658=CARTESIAN_POINT('Ctrl Pts',(0.753728118875441,2.70522619117216,-7.19340574734018));
#16659=CARTESIAN_POINT('Ctrl Pts',(0.766677009772667,2.69977763294854,-7.19528208283154));
#16660=CARTESIAN_POINT('Ctrl Pts',(0.779571505380582,2.69423287115845,-7.19715904078809));
#16661=CARTESIAN_POINT('Ctrl Pts',(0.863111309476644,2.65830992172418,-7.20931932256682));
#16662=CARTESIAN_POINT('Ctrl Pts',(0.944501853536966,2.61829878211877,-7.22152465472504));
#16663=CARTESIAN_POINT('Ctrl Pts',(1.02341032522997,2.57417267578142,-7.23379399917205));
#16664=CARTESIAN_POINT('Ctrl Pts',(1.06283985566158,2.55212343803384,-7.2399248299925));
#16665=CARTESIAN_POINT('Ctrl Pts',(1.10164917691728,2.52904610718385,-7.24607164384984));
#16666=CARTESIAN_POINT('Ctrl Pts',(1.13979350230052,2.50493366123382,-7.25223680653294));
#16667=CARTESIAN_POINT('Ctrl Pts',(1.21803336844641,2.45547533356318,-7.26488250148881));
#16668=CARTESIAN_POINT('Ctrl Pts',(1.29347831788253,2.40166348524667,-7.27760539418667));
#16669=CARTESIAN_POINT('Ctrl Pts',(1.36591536301843,2.3438254012589,-7.29042590061749));
#16670=CARTESIAN_POINT('Ctrl Pts',(1.44070207418648,2.284111202901,-7.30366227034614));
#16671=CARTESIAN_POINT('Ctrl Pts',(1.51228330084963,2.2201043116401,-7.31700268917746));
#16672=CARTESIAN_POINT('Ctrl Pts',(1.58037036975762,2.15214475623283,-7.33046962496539));
#16673=CARTESIAN_POINT('Ctrl Pts',(1.59177620103872,2.14076028579893,-7.33272558340116));
#16674=CARTESIAN_POINT('Ctrl Pts',(1.60308384365138,2.12926487077458,-7.33498509220474));
#16675=CARTESIAN_POINT('Ctrl Pts',(1.61429177548598,2.11766008923023,-7.33724825699667));
#16676=CARTESIAN_POINT('Ctrl Pts',(1.62281870648737,2.10883123721941,-7.33897005994038));
#16677=CARTESIAN_POINT('Ctrl Pts',(1.63128633441429,2.09994067011115,-7.34069366478485));
#16678=CARTESIAN_POINT('Ctrl Pts',(1.63968819128585,2.09099554765498,-7.342417896705));
#16679=CARTESIAN_POINT('Ctrl Pts',(1.70117666231045,2.02553122097506,-7.35503658160788));
#16680=CARTESIAN_POINT('Ctrl Pts',(1.7592398126132,1.95705067552547,-7.36770770253109));
#16681=CARTESIAN_POINT('Ctrl Pts',(1.81371002961462,1.88587543597805,-7.38045292702293));
#16682=CARTESIAN_POINT('Ctrl Pts',(1.86796536455275,1.81498097890537,-7.39314787229272));
#16683=CARTESIAN_POINT('Ctrl Pts',(1.91865635294755,1.74141204884235,-7.40591633761525));
#16684=CARTESIAN_POINT('Ctrl Pts',(1.96556921350444,1.66546856046612,-7.41877973511718));
#16685=CARTESIAN_POINT('Ctrl Pts',(2.01167925042842,1.59082469923926,-7.43142300024196));
#16686=CARTESIAN_POINT('Ctrl Pts',(2.05413950023982,1.51388595667896,-7.44415797618339));
#16687=CARTESIAN_POINT('Ctrl Pts',(2.09269735617246,1.43493390097717,-7.45700499449054));
#16688=CARTESIAN_POINT('Ctrl Pts',(2.11347557683795,1.39238788290419,-7.46392805011235));
#16689=CARTESIAN_POINT('Ctrl Pts',(2.13311968690992,1.34925723096723,-7.4708836424134));
#16690=CARTESIAN_POINT('Ctrl Pts',(2.15158382290223,1.30558696879693,-7.47787495307664));
#16691=CARTESIAN_POINT('Ctrl Pts',(2.15703256236091,1.29269993846108,-7.4799380786025));
#16692=CARTESIAN_POINT('Ctrl Pts',(2.16237928721174,1.27976400868627,-7.48200462000068));
#16693=CARTESIAN_POINT('Ctrl Pts',(2.16762028210649,1.26678646608345,-7.48407368538072));
#16694=CARTESIAN_POINT('Ctrl Pts',(2.1995233363961,1.1877893950085,-7.4966685278627));
#16695=CARTESIAN_POINT('Ctrl Pts',(2.22741547616661,1.107495335724,-7.50931797811288));
#16696=CARTESIAN_POINT('Ctrl Pts',(2.25111999516359,1.02617308053887,-7.52204418386055));
#16697=CARTESIAN_POINT('Ctrl Pts',(2.27447329643854,0.94605573557442,-7.53458183193307));
#16698=CARTESIAN_POINT('Ctrl Pts',(2.29376221982233,0.864939616052927,-7.54719397785926));
#16699=CARTESIAN_POINT('Ctrl Pts',(2.30876812899223,0.783083312057354,-7.55990179942786));
#16700=CARTESIAN_POINT('Ctrl Pts',(2.32333320662229,0.703631716775364,-7.57223630082726));
#16701=CARTESIAN_POINT('Ctrl Pts',(2.3338631266181,0.623482150018367,-7.58466093907477));
#16702=CARTESIAN_POINT('Ctrl Pts',(2.34011118715382,0.542883112509629,-7.59719507982054));
#16703=CARTESIAN_POINT('Ctrl Pts',(2.34523285688384,0.476814346319474,-7.6074695848261));
#16704=CARTESIAN_POINT('Ctrl Pts',(2.34747653436054,0.410443624436012,-7.61781766931087));
#16705=CARTESIAN_POINT('Ctrl Pts',(2.34668236863854,0.343918483395443,-7.62825));
#16706=CARTESIAN_POINT('Ctrl Pts',(-2.54872116535053,-0.00229165091991107,
-7.45095259589208));
#16707=CARTESIAN_POINT('Ctrl Pts',(-2.54884325303734,-0.00474672992966245,
-7.45085547912962));
#16708=CARTESIAN_POINT('Ctrl Pts',(-2.54896183162798,-0.00720206634178606,
-7.45075836090064));
#16709=CARTESIAN_POINT('Ctrl Pts',(-2.54907689689922,-0.00965765243994136,
-7.45066124109941));
#16710=CARTESIAN_POINT('Ctrl Pts',(-2.55333516415932,-0.100532525222233,
-7.44706708914183));
#16711=CARTESIAN_POINT('Ctrl Pts',(-2.55276357918561,-0.191272512218256,
-7.4434895845571));
#16712=CARTESIAN_POINT('Ctrl Pts',(-2.54727379502897,-0.281480958790373,
-7.43992360795864));
#16713=CARTESIAN_POINT('Ctrl Pts',(-2.54185772847415,-0.370478073522051,
-7.43640551580072));
#16714=CARTESIAN_POINT('Ctrl Pts',(-2.53165485646165,-0.45895878699389,
-7.43289864410887));
#16715=CARTESIAN_POINT('Ctrl Pts',(-2.51653085824622,-0.546550786572665,
-7.42939807697118));
#16716=CARTESIAN_POINT('Ctrl Pts',(-2.51229227063912,-0.571098948944002,
-7.42841702286919));
#16717=CARTESIAN_POINT('Ctrl Pts',(-2.50766684965454,-0.595577313484347,
-7.42743646394764));
#16718=CARTESIAN_POINT('Ctrl Pts',(-2.50265089448421,-0.619977651269288,
-7.42645629199643));
#16719=CARTESIAN_POINT('Ctrl Pts',(-2.48482398915618,-0.706697427840933,
-7.42297272167212));
#16720=CARTESIAN_POINT('Ctrl Pts',(-2.46206809920096,-0.792432697411164,
-7.41949403924777));
#16721=CARTESIAN_POINT('Ctrl Pts',(-2.43465304171894,-0.87692613469852,
-7.41601538697891));
#16722=CARTESIAN_POINT('Ctrl Pts',(-2.42548539819617,-0.905180888990806,
-7.41485211953139));
#16723=CARTESIAN_POINT('Ctrl Pts',(-2.41579632851701,-0.933296653750345,
-7.413688855456));
#16724=CARTESIAN_POINT('Ctrl Pts',(-2.40559471855271,-0.961263367130259,
-7.41252541310066));
#16725=CARTESIAN_POINT('Ctrl Pts',(-2.39903093632121,-0.979257332494453,
-7.41177684671888));
#16726=CARTESIAN_POINT('Ctrl Pts',(-2.39225293451855,-0.9971944580043,-7.41102800099647));
#16727=CARTESIAN_POINT('Ctrl Pts',(-2.385274720724,-1.0150428927436,-7.41028005192424));
#16728=CARTESIAN_POINT('Ctrl Pts',(-2.35172893850088,-1.10084417691406,
-7.40668449904645));
#16729=CARTESIAN_POINT('Ctrl Pts',(-2.3135230946086,-1.18470956672032,-7.40310499394341));
#16730=CARTESIAN_POINT('Ctrl Pts',(-2.27102243831346,-1.26637331179736,
-7.39953639877998));
#16731=CARTESIAN_POINT('Ctrl Pts',(-2.22895234350611,-1.34720974580101,
-7.39600395599104));
#16732=CARTESIAN_POINT('Ctrl Pts',(-2.1826732982571,-1.425889649158,-7.39248220321072));
#16733=CARTESIAN_POINT('Ctrl Pts',(-2.13248447954121,-1.50214210424881,
-7.38896615717692));
#16734=CARTESIAN_POINT('Ctrl Pts',(-2.08204495359797,-1.57877546174146,
-7.38543254750694));
#16735=CARTESIAN_POINT('Ctrl Pts',(-2.0276559274001,-1.65295784872659,-7.38190470173949));
#16736=CARTESIAN_POINT('Ctrl Pts',(-1.96957457655766,-1.72438946587683,
-7.37837756156043));
#16737=CARTESIAN_POINT('Ctrl Pts',(-1.94762706422866,-1.75138171511597,
-7.37704474213659));
#16738=CARTESIAN_POINT('Ctrl Pts',(-1.92515189733108,-1.77798086862864,
-7.37571202346358));
#16739=CARTESIAN_POINT('Ctrl Pts',(-1.90216149454643,-1.80416947090812,
-7.3743791326112));
#16740=CARTESIAN_POINT('Ctrl Pts',(-1.88977962052994,-1.81827378987677,
-7.37366128148147));
#16741=CARTESIAN_POINT('Ctrl Pts',(-1.87724828731966,-1.83225901324112,
-7.37294338041035));
#16742=CARTESIAN_POINT('Ctrl Pts',(-1.86456935020798,-1.8461223147433,-7.37222538676236));
#16743=CARTESIAN_POINT('Ctrl Pts',(-1.85494278415337,-1.85664811721949,
-7.37168024538196));
#16744=CARTESIAN_POINT('Ctrl Pts',(-1.84523713445571,-1.86709703864532,
-7.37113539153293));
#16745=CARTESIAN_POINT('Ctrl Pts',(-1.83545598652633,-1.87746553404443,
-7.37059094249616));
#16746=CARTESIAN_POINT('Ctrl Pts',(-1.77171523636253,-1.94503384806859,
-7.36704293460588));
#16747=CARTESIAN_POINT('Ctrl Pts',(-1.70473932291081,-2.00922447566438,
-7.36351026093116));
#16748=CARTESIAN_POINT('Ctrl Pts',(-1.63483249771768,-2.0697661447767,-7.35998798155957));
#16749=CARTESIAN_POINT('Ctrl Pts',(-1.56489051873596,-2.13033825825596,
-7.35646393095228));
#16750=CARTESIAN_POINT('Ctrl Pts',(-1.49201405105733,-2.18725850548537,
-7.35295028510463));
#16751=CARTESIAN_POINT('Ctrl Pts',(-1.41646639948432,-2.24022488946181,
-7.3494420966481));
#16752=CARTESIAN_POINT('Ctrl Pts',(-1.34208268676144,-2.29237523705884,
-7.34598795774511));
#16753=CARTESIAN_POINT('Ctrl Pts',(-1.26510879589927,-2.34069325196222,
-7.34253910936801));
#16754=CARTESIAN_POINT('Ctrl Pts',(-1.18576568003122,-2.38485106755256,
-7.33909082931102));
#16755=CARTESIAN_POINT('Ctrl Pts',(-1.15640740682169,-2.40119019414539,
-7.33781490830756));
#16756=CARTESIAN_POINT('Ctrl Pts',(-1.12672450477203,-2.41695929561798,
-7.33653906511412));
#16757=CARTESIAN_POINT('Ctrl Pts',(-1.09672736577269,-2.43214008652495,
-7.33526306050453));
#16758=CARTESIAN_POINT('Ctrl Pts',(-1.08062679344899,-2.44028817764571,
-7.3345781817065));
#16759=CARTESIAN_POINT('Ctrl Pts',(-1.06443568717334,-2.448266767796,-7.33389325640666));
#16760=CARTESIAN_POINT('Ctrl Pts',(-1.04815561213944,-2.45607290918114,
-7.33320824761425));
#16761=CARTESIAN_POINT('Ctrl Pts',(-1.0370323350443,-2.46140641492298,-7.33274021889849));
#16762=CARTESIAN_POINT('Ctrl Pts',(-1.02586911010053,-2.4666586051756,-7.33227221874498));
#16763=CARTESIAN_POINT('Ctrl Pts',(-1.01467488717969,-2.47182484947527,
-7.3318045847467));
#16764=CARTESIAN_POINT('Ctrl Pts',(-0.964722922882861,-2.49487817373284,
-7.32971786225141));
#16765=CARTESIAN_POINT('Ctrl Pts',(-0.91410779186745,-2.51624284380486,
-7.32763648114457));
#16766=CARTESIAN_POINT('Ctrl Pts',(-0.8628861291915,-2.53585963668761,-7.32555943799463));
#16767=CARTESIAN_POINT('Ctrl Pts',(-0.779322982596467,-2.56786252089221,
-7.32217094468622));
#16768=CARTESIAN_POINT('Ctrl Pts',(-0.694146848480023,-2.59521630651244,
-7.31879399673727));
#16769=CARTESIAN_POINT('Ctrl Pts',(-0.607724558635994,-2.61805914565455,
-7.31542423731298));
#16770=CARTESIAN_POINT('Ctrl Pts',(-0.519092379891881,-2.64148609494646,
-7.31196831037378));
#16771=CARTESIAN_POINT('Ctrl Pts',(-0.429148743139305,-2.66016857380842,
-7.30851994429254));
#16772=CARTESIAN_POINT('Ctrl Pts',(-0.338268208316806,-2.6742053818501,
-7.30507443939171));
#16773=CARTESIAN_POINT('Ctrl Pts',(-0.248676928654702,-2.68804306004249,
-7.30167781332925));
#16774=CARTESIAN_POINT('Ctrl Pts',(-0.158174285448021,-2.69736576180666,
-7.29828396784411));
#16775=CARTESIAN_POINT('Ctrl Pts',(-0.0671111582030917,-2.70222088552231,
-7.2948884004473));
#16776=CARTESIAN_POINT('Ctrl Pts',(-0.045603233936238,-2.70336760249044,
-7.29408641166629));
#16777=CARTESIAN_POINT('Ctrl Pts',(-0.0240569840929646,-2.70426498015991,
-7.29328406477781));
#16778=CARTESIAN_POINT('Ctrl Pts',(-0.00251467253543246,-2.70491251705096,
-7.29248269889014));
#16779=CARTESIAN_POINT('Ctrl Pts',(0.0913505575722242,-2.70773399696131,
-7.28899094763375));
#16780=CARTESIAN_POINT('Ctrl Pts',(0.185240927263786,-2.7058247172191,-7.28551403200604));
#16781=CARTESIAN_POINT('Ctrl Pts',(0.278764535523396,-2.69931752457491,
-7.28204725167995));
#16782=CARTESIAN_POINT('Ctrl Pts',(0.373533208232459,-2.69272370274288,
-7.27853431867628));
#16783=CARTESIAN_POINT('Ctrl Pts',(0.467926227188296,-2.68140873303817,
-7.27503179262975));
#16784=CARTESIAN_POINT('Ctrl Pts',(0.561545441819487,-2.66545794439719,
-7.27153478297901));
#16785=CARTESIAN_POINT('Ctrl Pts',(0.654945657927808,-2.64954446860021,
-7.26804595369969));
#16786=CARTESIAN_POINT('Ctrl Pts',(0.747576659440711,-2.62901672313918,
-7.26456261503792));
#16787=CARTESIAN_POINT('Ctrl Pts',(0.839038170974715,-2.60390818657947,
-7.26107991067285));
#16788=CARTESIAN_POINT('Ctrl Pts',(0.879163798785432,-2.59289267004177,
-7.25955199257064));
#16789=CARTESIAN_POINT('Ctrl Pts',(0.919064181798801,-2.58099482605824,
-7.25802419655261));
#16790=CARTESIAN_POINT('Ctrl Pts',(0.9587044796514,-2.56821443729529,-7.25649611254898));
#16791=CARTESIAN_POINT('Ctrl Pts',(0.977255688629643,-2.56223336057265,
-7.25578098659828));
#16792=CARTESIAN_POINT('Ctrl Pts',(0.995749923609562,-2.55605896850107,
-7.25506579757489));
#16793=CARTESIAN_POINT('Ctrl Pts',(1.01418354344848,-2.54969110077333,-7.25435050344838));
#16794=CARTESIAN_POINT('Ctrl Pts',(1.0270766997497,-2.54523717828622,-7.25385020024938));
#16795=CARTESIAN_POINT('Ctrl Pts',(1.03993108370967,-2.54069175052625,-7.25335019936401));
#16796=CARTESIAN_POINT('Ctrl Pts',(1.05274516772751,-2.53605528929552,-7.2528505022789));
#16797=CARTESIAN_POINT('Ctrl Pts',(1.14311406147389,-2.50335752707269,-7.24932648349403));
#16798=CARTESIAN_POINT('Ctrl Pts',(1.23148546628133,-2.46613421062177,-7.24581732198645));
#16799=CARTESIAN_POINT('Ctrl Pts',(1.31746058766075,-2.42447327586601,-7.24231818331382));
#16800=CARTESIAN_POINT('Ctrl Pts',(1.40202683996985,-2.38349503630713,-7.2388763848132));
#16801=CARTESIAN_POINT('Ctrl Pts',(1.48427560644325,-2.33822317751169,-7.23544428335181));
#16802=CARTESIAN_POINT('Ctrl Pts',(1.56381530896657,-2.28869332060664,-7.2320172782791));
#16803=CARTESIAN_POINT('Ctrl Pts',(1.62076292161253,-2.25323169558218,-7.22956366390508));
#16804=CARTESIAN_POINT('Ctrl Pts',(1.676321640262,-2.21558640461195,-7.22711266196708));
#16805=CARTESIAN_POINT('Ctrl Pts',(1.7303399838677,-2.17575595906912,-7.22466258399285));
#16806=CARTESIAN_POINT('Ctrl Pts',(1.77747898896718,-2.14099799630627,-7.22252452809531));
#16807=CARTESIAN_POINT('Ctrl Pts',(1.82344488788193,-2.10457574306011,-7.22038717580978));
#16808=CARTESIAN_POINT('Ctrl Pts',(1.86820503283264,-2.06657448017728,-7.21824940508842));
#16809=CARTESIAN_POINT('Ctrl Pts',(1.8902908163544,-2.04782369939881,-7.21719457514041));
#16810=CARTESIAN_POINT('Ctrl Pts',(1.9120829551215,-2.02868838834088,-7.21613964331649));
#16811=CARTESIAN_POINT('Ctrl Pts',(1.93357702544331,-2.0091783017074,-7.21508447482116));
#16812=CARTESIAN_POINT('Ctrl Pts',(1.94403188955915,-1.99968846094725,-7.21457123358427));
#16813=CARTESIAN_POINT('Ctrl Pts',(1.95440865049196,-1.99011682212725,-7.214058308234));
#16814=CARTESIAN_POINT('Ctrl Pts',(1.96470674377952,-1.98046518688763,-7.21354570043154));
#16815=CARTESIAN_POINT('Ctrl Pts',(2.03231051209255,-1.91710521389451,-7.21018059019757));
#16816=CARTESIAN_POINT('Ctrl Pts',(2.09653100691307,-1.85029719530032,-7.20682892803937));
#16817=CARTESIAN_POINT('Ctrl Pts',(2.15728945535032,-1.78043655567924,-7.2034865054898));
#16818=CARTESIAN_POINT('Ctrl Pts',(2.22026134829767,-1.70803087659091,-7.20002231770374));
#16819=CARTESIAN_POINT('Ctrl Pts',(2.27951493325531,-1.63234557769656,-7.19656805499097));
#16820=CARTESIAN_POINT('Ctrl Pts',(2.33492983764645,-1.55377538415515,-7.19311903197858));
#16821=CARTESIAN_POINT('Ctrl Pts',(2.38183708392325,-1.48726779997799,-7.19019952550943));
#16822=CARTESIAN_POINT('Ctrl Pts',(2.42599342603758,-1.41869208607858,-7.18728377337642));
#16823=CARTESIAN_POINT('Ctrl Pts',(2.4673039324097,-1.34826833541749,-7.18436893384037));
#16824=CARTESIAN_POINT('Ctrl Pts',(2.50345062548531,-1.28664755358903,-7.18181844924633));
#16825=CARTESIAN_POINT('Ctrl Pts',(2.53741825419599,-1.22361145783562,-7.17926866335933));
#16826=CARTESIAN_POINT('Ctrl Pts',(2.5691287863742,-1.15929983468204,-7.17671767243616));
#16827=CARTESIAN_POINT('Ctrl Pts',(2.57735307324704,-1.14262029000899,-7.17605606004049));
#16828=CARTESIAN_POINT('Ctrl Pts',(2.58542693226734,-1.12585155808721,-7.17539423637559));
#16829=CARTESIAN_POINT('Ctrl Pts',(2.5933377461211,-1.10902032020036,-7.17473311722116));
#16830=CARTESIAN_POINT('Ctrl Pts',(2.6349885962116,-1.02040296944197,-7.17125229017833));
#16831=CARTESIAN_POINT('Ctrl Pts',(2.67218718831404,-0.929929724788019,
-7.1677859564656));
#16832=CARTESIAN_POINT('Ctrl Pts',(2.70481573622773,-0.838000353098113,
-7.16432946488494));
#16833=CARTESIAN_POINT('Ctrl Pts',(2.73755084161654,-0.745770760823376,
-7.1608616851827));
#16834=CARTESIAN_POINT('Ctrl Pts',(2.76568644862227,-0.652074656152445,
-7.15740381200185));
#16835=CARTESIAN_POINT('Ctrl Pts',(2.78906022130522,-0.557287603626856,
-7.15395114842608));
#16836=CARTESIAN_POINT('Ctrl Pts',(2.81210271895143,-0.463843962142935,
-7.15054741923795));
#16837=CARTESIAN_POINT('Ctrl Pts',(2.83051771268829,-0.369339210646432,
-7.14714875303053));
#16838=CARTESIAN_POINT('Ctrl Pts',(2.84410218393759,-0.27411879745952,-7.14375064977776));
#16839=CARTESIAN_POINT('Ctrl Pts',(2.85077740762626,-0.227328786565033,
-7.14208086823727));
#16840=CARTESIAN_POINT('Ctrl Pts',(2.85628549214726,-0.180365830909598,
-7.14041122262811));
#16841=CARTESIAN_POINT('Ctrl Pts',(2.860597698937,-0.133270579992977,-7.13874117902033));
#16842=CARTESIAN_POINT('Ctrl Pts',(2.86229734993567,-0.114708044809467,
-7.13808293338783));
#16843=CARTESIAN_POINT('Ctrl Pts',(2.86381118226309,-0.0961249578213986,
-7.13742462592495));
#16844=CARTESIAN_POINT('Ctrl Pts',(2.86513729621133,-0.0775238157094563,
-7.13676622393794));
#16845=CARTESIAN_POINT('Ctrl Pts',(2.86615128521417,-0.0633007894251151,
-7.13626278878806));
#16846=CARTESIAN_POINT('Ctrl Pts',(2.86705513484125,-0.0490720314096428,
-7.13575946921485));
#16847=CARTESIAN_POINT('Ctrl Pts',(2.86784786602706,-0.034846719776545,
-7.13525653467227));
#16848=CARTESIAN_POINT('Ctrl Pts',(2.87331995000557,0.0633481049887041,
-7.1317848659629));
#16849=CARTESIAN_POINT('Ctrl Pts',(2.87350981423829,0.161493285384653,-7.12832744179556));
#16850=CARTESIAN_POINT('Ctrl Pts',(2.86825916071671,0.259214272665054,-7.12487964669447));
#16851=CARTESIAN_POINT('Ctrl Pts',(2.86769353153745,0.26974131308102,-7.12450823130679));
#16852=CARTESIAN_POINT('Ctrl Pts',(2.86706471810811,0.280263443667678,-7.12413692766231));
#16853=CARTESIAN_POINT('Ctrl Pts',(2.86637248699574,0.290780204225716,-7.12376572999106));
#16854=CARTESIAN_POINT('Ctrl Pts',(2.86009088031278,0.386213871138418,-7.12039732061053));
#16855=CARTESIAN_POINT('Ctrl Pts',(2.8485916250155,0.481205266105106,-7.11703763763718));
#16856=CARTESIAN_POINT('Ctrl Pts',(2.83214991077614,0.57546107308452,-7.11368236954826));
#16857=CARTESIAN_POINT('Ctrl Pts',(2.8153985065753,0.671492247085209,-7.11026390288831));
#16858=CARTESIAN_POINT('Ctrl Pts',(2.79351642813581,0.766760638665728,-7.10685001899331));
#16859=CARTESIAN_POINT('Ctrl Pts',(2.76674040525016,0.860950212594716,-7.10343615809206));
#16860=CARTESIAN_POINT('Ctrl Pts',(2.75761693499742,0.89304369337525,-7.10227294358061));
#16861=CARTESIAN_POINT('Ctrl Pts',(2.74792484490626,0.92501182174776,-7.10110973173872));
#16862=CARTESIAN_POINT('Ctrl Pts',(2.73767218810561,0.956841690536304,-7.09994634218776));
#16863=CARTESIAN_POINT('Ctrl Pts',(2.73046159724209,0.97922731852874,-7.09912814196611));
#16864=CARTESIAN_POINT('Ctrl Pts',(2.72297372710465,1.00154455613911,-7.09830985384657));
#16865=CARTESIAN_POINT('Ctrl Pts',(2.71521119495974,1.0237888281201,-7.09749141508282));
#16866=CARTESIAN_POINT('Ctrl Pts',(2.7105158736684,1.03724371653708,-7.09699636618881));
#16867=CARTESIAN_POINT('Ctrl Pts',(2.70572160653792,1.05066736008874,-7.09650142908722));
#16868=CARTESIAN_POINT('Ctrl Pts',(2.70083194831629,1.06405145610732,-7.09600686216269));
#16869=CARTESIAN_POINT('Ctrl Pts',(2.666977201111,1.15671952547791,-7.09258260683707));
#16870=CARTESIAN_POINT('Ctrl Pts',(2.62851664991674,1.24759973569772,-7.08917213696652));
#16871=CARTESIAN_POINT('Ctrl Pts',(2.58574587816133,1.33638733434256,-7.08577102509522));
#16872=CARTESIAN_POINT('Ctrl Pts',(2.54241251743573,1.426342808189,-7.08232517641075));
#16873=CARTESIAN_POINT('Ctrl Pts',(2.49465442167471,1.5141510805358,-7.07888893352709));
#16874=CARTESIAN_POINT('Ctrl Pts',(2.44272590781198,1.59948420693675,-7.07545769196954));
#16875=CARTESIAN_POINT('Ctrl Pts',(2.39086769403728,1.68470181055743,-7.0720310955783));
#16876=CARTESIAN_POINT('Ctrl Pts',(2.33484985166447,1.76745178247923,-7.06860948698087));
#16877=CARTESIAN_POINT('Ctrl Pts',(2.27487983880247,1.84738429843036,-7.06518828037767));
#16878=CARTESIAN_POINT('Ctrl Pts',(2.23288468478585,1.90335857887663,-7.06279251470467));
#16879=CARTESIAN_POINT('Ctrl Pts',(2.18895051670804,1.95795077859895,-7.06039694616037));
#16880=CARTESIAN_POINT('Ctrl Pts',(2.14313711407334,2.01103068470338,-7.058));
#16881=CARTESIAN_POINT('Ctrl Pts',(0.545102916878531,2.89105980740809,-7.95748399100539));
#16882=CARTESIAN_POINT('Ctrl Pts',(-0.418551816366991,3.07275477082944,
-7.90443409773202));
#16883=CARTESIAN_POINT('Ctrl Pts',(-2.52507517261166,2.39323450065356,-7.79833431118528));
#16884=CARTESIAN_POINT('Ctrl Pts',(-3.38010884006162,-0.837958625187954,
-7.63918463136517));
#16885=CARTESIAN_POINT('Ctrl Pts',(-1.12023390429596,-3.29384205719836,
-7.48003495154506));
#16886=CARTESIAN_POINT('Ctrl Pts',(2.16577264269164,-2.72400316663615,-7.32088527172496));
#16887=CARTESIAN_POINT('Ctrl Pts',(3.4626380957396,0.351377294665846,-7.16173559190485));
#16888=CARTESIAN_POINT('Ctrl Pts',(1.57515132522855,3.10306773376032,-7.00258591208474));
#16889=CARTESIAN_POINT('Ctrl Pts',(-1.75990653256836,3.00232659448819,-6.84343623226463));
#16890=CARTESIAN_POINT('Ctrl Pts',(-3.47728821638593,0.141248766687278,
-6.68428655244452));
#16891=CARTESIAN_POINT('Ctrl Pts',(-1.99771660476884,-2.84959140114192,
-6.52513687262442));
#16892=CARTESIAN_POINT('Ctrl Pts',(1.3183600049385,-3.22073768325123,-6.3659871928043));
#16893=CARTESIAN_POINT('Ctrl Pts',(3.42245518605895,-0.630906395973156,
-6.20683751298421));
#16894=CARTESIAN_POINT('Ctrl Pts',(2.38013079602577,2.53892891859366,-6.04768783316409));
#16895=CARTESIAN_POINT('Ctrl Pts',(-0.850331682068317,3.37463293930467,
-5.88853815334399));
#16896=CARTESIAN_POINT('Ctrl Pts',(-3.29905605961118,1.10789918584346,-5.72938847352388));
#16897=CARTESIAN_POINT('Ctrl Pts',(-2.71482419166764,-2.17736841611413,
-5.57023879370378));
#16898=CARTESIAN_POINT('Ctrl Pts',(0.365251897578816,-3.46089570740757,
-5.41108911388365));
#16899=CARTESIAN_POINT('Ctrl Pts',(3.10953820283011,-1.56268354366004,-5.25193943406356));
#16900=CARTESIAN_POINT('Ctrl Pts',(2.9951020675602,1.77216542315489,-5.09278975424344));
#16901=CARTESIAN_POINT('Ctrl Pts',(0.127149812658285,3.47779244265733,-4.93364007442334));
#16902=CARTESIAN_POINT('Ctrl Pts',(-2.85769643090647,1.9861466101059,-4.77449039460323));
#16903=CARTESIAN_POINT('Ctrl Pts',(-3.21534873908604,-1.3314426796523,-4.61534071478312));
#16904=CARTESIAN_POINT('Ctrl Pts',(-0.617003224446478,-3.42498383104617,
-4.45619103496301));
#16905=CARTESIAN_POINT('Ctrl Pts',(2.54857788636968,-2.36980124815908,-4.29704135514291));
#16906=CARTESIAN_POINT('Ctrl Pts',(3.371150073419,0.864033777125352,-4.1378916753228));
#16907=CARTESIAN_POINT('Ctrl Pts',(1.09449005337646,3.30352822398509,-3.97874199550269));
#16908=CARTESIAN_POINT('Ctrl Pts',(-2.1883781623069,2.70595790881245,-3.81959231568258));
#16909=CARTESIAN_POINT('Ctrl Pts',(-3.45938338148725,-0.379307024135721,
-3.66044263586248));
#16910=CARTESIAN_POINT('Ctrl Pts',(-1.55004000081492,-3.11585994835756,
-3.50129295604237));
#16911=CARTESIAN_POINT('Ctrl Pts',(1.78431673513788,-2.98787899886338,-3.34214327622227));
#16912=CARTESIAN_POINT('Ctrl Pts',(3.47828021156799,-0.113022200762772,
-3.18299359640215));
#16913=CARTESIAN_POINT('Ctrl Pts',(1.97452245968913,2.86574046369287,-3.02384391658205));
#16914=CARTESIAN_POINT('Ctrl Pts',(-1.34449219737245,3.20991392615656,-2.86469423676194));
#16915=CARTESIAN_POINT('Ctrl Pts',(-3.42746184614662,0.603086217463922,
-2.70554455694183));
#16916=CARTESIAN_POINT('Ctrl Pts',(-2.35942946044921,-2.55818307933608,
-2.54639487712173));
#16917=CARTESIAN_POINT('Ctrl Pts',(0.877719845461013,-3.36761213384782,
-2.38724519730161));
#16918=CARTESIAN_POINT('Ctrl Pts',(3.30794705758641,-1.08106325192158,-2.22809551748151));
#16919=CARTESIAN_POINT('Ctrl Pts',(2.69704588622583,2.19935329862247,-2.0689458376614));
#16920=CARTESIAN_POINT('Ctrl Pts',(-0.393354403714323,3.45781071965196,
-1.90979615784129));
#16921=CARTESIAN_POINT('Ctrl Pts',(-3.12213281863858,1.53737732643667,-1.75064647802119));
#16922=CARTESIAN_POINT('Ctrl Pts',(-2.98060194491491,-1.79645104940419,
-1.59149679820108));
#16923=CARTESIAN_POINT('Ctrl Pts',(-0.0989016115630054,-3.47868671450324,
-1.43234711838097));
#16924=CARTESIAN_POINT('Ctrl Pts',(2.87375418364955,-1.96291147173372,-1.27319743856086));
#16925=CARTESIAN_POINT('Ctrl Pts',(3.20439368630738,1.35760711787367,-1.11404775874076));
#16926=CARTESIAN_POINT('Ctrl Pts',(0.58922140315462,3.42971561441151,-0.954898078920646));
#16927=CARTESIAN_POINT('Ctrl Pts',(-2.56786503715982,2.34933985115096,-0.795748399100539));
#16928=CARTESIAN_POINT('Ctrl Pts',(-3.36379079604088,-0.89200665476552,
-0.636598719280432));
#16929=CARTESIAN_POINT('Ctrl Pts',(-1.06805538932566,-3.31112929125929,
-0.477449039460324));
#16930=CARTESIAN_POINT('Ctrl Pts',(2.21113366938903,-2.69038999483046,-0.318299359640216));
#16931=CARTESIAN_POINT('Ctrl Pts',(3.45452145423158,0.412137749680903,-0.159149679820109));
#16932=CARTESIAN_POINT('Ctrl Pts',(2.17043456109762,2.21499916944277,-0.0530498932733694));
#16933=CARTESIAN_POINT('Ctrl Pts',(1.28892185405323,2.64462557919718,0.));
#16934=CARTESIAN_POINT('Ctrl Pts',(0.509883685250385,2.70426773226936,-7.84773932733692));
#16935=CARTESIAN_POINT('Ctrl Pts',(-0.391509082027172,2.8742233400493,-7.79468943406355));
#16936=CARTESIAN_POINT('Ctrl Pts',(-2.36192945346575,2.23860703928967,-7.68858964751681));
#16937=CARTESIAN_POINT('Ctrl Pts',(-3.16171918834565,-0.783817915238558,
-7.52943996769672));
#16938=CARTESIAN_POINT('Ctrl Pts',(-1.04785532012138,-3.0810261232399,-7.37029028787659));
#16939=CARTESIAN_POINT('Ctrl Pts',(2.02584154712231,-2.54800466156315,-7.2111406080565));
#16940=CARTESIAN_POINT('Ctrl Pts',(3.23891620880379,0.32867472246064,-7.05199092823639));
#16941=CARTESIAN_POINT('Ctrl Pts',(1.47338041618576,2.90257777509537,-6.89284124841627));
#16942=CARTESIAN_POINT('Ctrl Pts',(-1.64619854478261,2.80834554525786,-6.73369156859618));
#16943=CARTESIAN_POINT('Ctrl Pts',(-3.25261978160301,0.132122649623666,
-6.57454188877606));
#16944=CARTESIAN_POINT('Ctrl Pts',(-1.86864365055748,-2.66547860978671,
-6.41539220895596));
#16945=CARTESIAN_POINT('Ctrl Pts',(1.23318044536269,-3.01264504061877,-6.25624252913584));
#16946=CARTESIAN_POINT('Ctrl Pts',(3.20132952666057,-0.590143380756329,
-6.09709284931574));
#16947=CARTESIAN_POINT('Ctrl Pts',(2.22634996819508,2.3748881055608,-5.93794316949563));
#16948=CARTESIAN_POINT('Ctrl Pts',(-0.795391545913839,3.15659708686432,
-5.77879348967553));
#16949=CARTESIAN_POINT('Ctrl Pts',(-3.08590324769261,1.03631755081884,-5.61964380985541));
#16950=CARTESIAN_POINT('Ctrl Pts',(-2.53941874239294,-2.0366881148124,-5.46049413003531));
#16951=CARTESIAN_POINT('Ctrl Pts',(0.34165288391529,-3.23728639660436,-5.3013444502152));
#16952=CARTESIAN_POINT('Ctrl Pts',(2.9086301855897,-1.4617181810074,-5.1421947703951));
#16953=CARTESIAN_POINT('Ctrl Pts',(2.80158779676639,1.65766538547598,-4.98304509057499));
#16954=CARTESIAN_POINT('Ctrl Pts',(0.118934632432992,3.25309142969275,-4.82389541075487));
#16955=CARTESIAN_POINT('Ctrl Pts',(-2.67305997161298,1.85782119605504,-4.66474573093477));
#16956=CARTESIAN_POINT('Ctrl Pts',(-3.00760427744274,-1.24541784529113,
-4.50559605111466));
#16957=CARTESIAN_POINT('Ctrl Pts',(-0.577138496513027,-3.20369479528205,
-4.34644637129456));
#16958=CARTESIAN_POINT('Ctrl Pts',(2.38391365118927,-2.21668781492061,-4.18729669147445));
#16959=CARTESIAN_POINT('Ctrl Pts',(3.153339249788,0.808208345286956,-4.02814701165434));
#16960=CARTESIAN_POINT('Ctrl Pts',(1.02377478565178,3.09008646444198,-3.86899733183423));
#16961=CARTESIAN_POINT('Ctrl Pts',(-2.04698651863418,2.53112531222279,-3.70984765201412));
#16962=CARTESIAN_POINT('Ctrl Pts',(-3.23587178242843,-0.354799905337474,
-3.55069797219402));
#16963=CARTESIAN_POINT('Ctrl Pts',(-1.44989154053112,-2.91454348160582,
-3.39154829237391));
#16964=CARTESIAN_POINT('Ctrl Pts',(1.66903159824548,-2.79483141228941,-3.2323986125538));
#16965=CARTESIAN_POINT('Ctrl Pts',(3.25354768373583,-0.105719808967507,
-3.0732489327337));
#16966=CARTESIAN_POINT('Ctrl Pts',(1.84694808481515,2.68058427749065,-2.91409925291358));
#16967=CARTESIAN_POINT('Ctrl Pts',(-1.25762423050732,3.00252060909438,-2.75494957309348));
#16968=CARTESIAN_POINT('Ctrl Pts',(-3.20601270522604,0.564120670726008,
-2.59579989327337));
#16969=CARTESIAN_POINT('Ctrl Pts',(-2.20698615092947,-2.39289825030919,
-2.43665021345326));
#16970=CARTESIAN_POINT('Ctrl Pts',(0.82101015342905,-3.15002989735035,-2.27750053363316));
#16971=CARTESIAN_POINT('Ctrl Pts',(3.0942197961329,-1.01121549309444,-2.11835085381304));
#16972=CARTESIAN_POINT('Ctrl Pts',(2.52278909757635,2.05725254873131,-1.95920117399294));
#16973=CARTESIAN_POINT('Ctrl Pts',(-0.367939680315494,3.23440073065564,
-1.80005149417283));
#16974=CARTESIAN_POINT('Ctrl Pts',(-2.92041106021703,1.43804700461472,-1.64090181435273));
#16975=CARTESIAN_POINT('Ctrl Pts',(-2.78802453056098,-1.68038191152489,
-1.48175213453262));
#16976=CARTESIAN_POINT('Ctrl Pts',(-0.0925115544596916,-3.25392792241787,
-1.32260245471251));
#16977=CARTESIAN_POINT('Ctrl Pts',(2.68808022905787,-1.8360872856068,-1.1634527748924));
#16978=CARTESIAN_POINT('Ctrl Pts',(2.99735703328033,1.26989179281504,-1.00430309507229));
#16979=CARTESIAN_POINT('Ctrl Pts',(0.551151665430965,3.20812085697687,-0.845153415252187));
#16980=CARTESIAN_POINT('Ctrl Pts',(-2.4019546544904,2.19754843373437,-0.686003735432076));
#16981=CARTESIAN_POINT('Ctrl Pts',(-3.14645545710565,-0.834373888520336,
-0.526854055611971));
#16982=CARTESIAN_POINT('Ctrl Pts',(-0.9990480716548,-3.0971964249166,-0.367704375791862));
#16983=CARTESIAN_POINT('Ctrl Pts',(2.0682717868863,-2.51656324493786,-0.208554695971755));
#16984=CARTESIAN_POINT('Ctrl Pts',(3.23132398547161,0.385509429744861,-0.049405016151647));
#16985=CARTESIAN_POINT('Ctrl Pts',(2.03020225784972,2.07188753604432,0.0566947703950921));
#16986=CARTESIAN_POINT('Ctrl Pts',(1.20564430054384,2.47375567929493,0.109744663668461));
#16987=CARTESIAN_POINT('Ctrl Pts',(0.474664453622239,2.51747565713063,-7.73799466366846));
#16988=CARTESIAN_POINT('Ctrl Pts',(-0.364466347687353,2.67569190926916,
-7.6849447703951));
#16989=CARTESIAN_POINT('Ctrl Pts',(-2.19878373431984,2.08397957792578,-7.57884498384835));
#16990=CARTESIAN_POINT('Ctrl Pts',(-2.94332953662968,-0.729677205289159,
-7.41969530402826));
#16991=CARTESIAN_POINT('Ctrl Pts',(-0.975476735946805,-2.86821018928144,
-7.26054562420813));
#16992=CARTESIAN_POINT('Ctrl Pts',(1.88591045155299,-2.37200615649015,-7.10139594438804));
#16993=CARTESIAN_POINT('Ctrl Pts',(3.01519432186797,0.305972150255433,-6.94224626456792));
#16994=CARTESIAN_POINT('Ctrl Pts',(1.37160950714298,2.70208781643043,-6.78309658474782));
#16995=CARTESIAN_POINT('Ctrl Pts',(-1.53249055699685,2.61436449602753,-6.62394690492771));
#16996=CARTESIAN_POINT('Ctrl Pts',(-3.02795134682008,0.12299653256005,-6.4647972251076));
#16997=CARTESIAN_POINT('Ctrl Pts',(-1.73957069634612,-2.48136581843149,
-6.3056475452875));
#16998=CARTESIAN_POINT('Ctrl Pts',(1.14800088578687,-2.80455239798632,-6.14649786546738));
#16999=CARTESIAN_POINT('Ctrl Pts',(2.98020386726219,-0.549380365539499,
-5.98734818564728));
#17000=CARTESIAN_POINT('Ctrl Pts',(2.07256914036438,2.21084729252794,-5.82819850582717));
#17001=CARTESIAN_POINT('Ctrl Pts',(-0.740451409759363,2.93856123442398,
-5.66904882600706));
#17002=CARTESIAN_POINT('Ctrl Pts',(-2.87275043577405,0.964735915794223,
-5.50989914618696));
#17003=CARTESIAN_POINT('Ctrl Pts',(-2.36401329311824,-1.89600781351067,
-5.35074946636685));
#17004=CARTESIAN_POINT('Ctrl Pts',(0.318053870251765,-3.01367708580114,
-5.19159978654674));
#17005=CARTESIAN_POINT('Ctrl Pts',(2.70772216834929,-1.36075281835476,-5.03245010672663));
#17006=CARTESIAN_POINT('Ctrl Pts',(2.60807352597257,1.54316534779707,-4.87330042690653));
#17007=CARTESIAN_POINT('Ctrl Pts',(0.1107194522077,3.02839041672818,-4.71415074708642));
#17008=CARTESIAN_POINT('Ctrl Pts',(-2.48842351231948,1.72949578200417,-4.55500106726631));
#17009=CARTESIAN_POINT('Ctrl Pts',(-2.79985981579943,-1.15939301092996,
-4.3958513874462));
#17010=CARTESIAN_POINT('Ctrl Pts',(-0.537273768579575,-2.98240575951794,
-4.23670170762609));
#17011=CARTESIAN_POINT('Ctrl Pts',(2.21924941600886,-2.06357438168214,-4.07755202780599));
#17012=CARTESIAN_POINT('Ctrl Pts',(2.935528426157,0.752382913448559,-3.91840234798588));
#17013=CARTESIAN_POINT('Ctrl Pts',(0.953059517927111,2.87664470489887,-3.75925266816577));
#17014=CARTESIAN_POINT('Ctrl Pts',(-1.90559487496145,2.35629271563314,-3.60010298834566));
#17015=CARTESIAN_POINT('Ctrl Pts',(-3.01236018336962,-0.330292786539225,
-3.44095330852556));
#17016=CARTESIAN_POINT('Ctrl Pts',(-1.34974308024733,-2.71322701485407,
-3.28180362870545));
#17017=CARTESIAN_POINT('Ctrl Pts',(1.55374646135307,-2.60178382571544,-3.12265394888534));
#17018=CARTESIAN_POINT('Ctrl Pts',(3.02881515590367,-0.0984174171722393,
-2.96350426906523));
#17019=CARTESIAN_POINT('Ctrl Pts',(1.71937370994117,2.49542809128842,-2.80435458924512));
#17020=CARTESIAN_POINT('Ctrl Pts',(-1.17075626364219,2.7951272920322,-2.64520490942502));
#17021=CARTESIAN_POINT('Ctrl Pts',(-2.98456356430545,0.525155123988089,
-2.48605522960491));
#17022=CARTESIAN_POINT('Ctrl Pts',(-2.05454284140974,-2.22761342128229,
-2.3269055497848));
#17023=CARTESIAN_POINT('Ctrl Pts',(0.764300461397087,-2.93244766085287,
-2.16775586996469));
#17024=CARTESIAN_POINT('Ctrl Pts',(2.8804925346794,-0.941367734267301,-2.00860619014458));
#17025=CARTESIAN_POINT('Ctrl Pts',(2.34853230892687,1.91515179884014,-1.84945651032448));
#17026=CARTESIAN_POINT('Ctrl Pts',(-0.342524956916667,3.01099074165932,
-1.69030683050437));
#17027=CARTESIAN_POINT('Ctrl Pts',(-2.71868930179547,1.33871668279276,-1.53115715068426));
#17028=CARTESIAN_POINT('Ctrl Pts',(-2.59544711620706,-1.56431277364559,
-1.37200747086416));
#17029=CARTESIAN_POINT('Ctrl Pts',(-0.0861214973563786,-3.0291691303325,
-1.21285779104405));
#17030=CARTESIAN_POINT('Ctrl Pts',(2.5024062744662,-1.70926309947988,-1.05370811122394));
#17031=CARTESIAN_POINT('Ctrl Pts',(2.79032038025327,1.18217646775642,-0.894558431403832));
#17032=CARTESIAN_POINT('Ctrl Pts',(0.513081927707314,2.98652609954223,-0.735408751583725));
#17033=CARTESIAN_POINT('Ctrl Pts',(-2.23604427182097,2.04575701631777,-0.576259071763615));
#17034=CARTESIAN_POINT('Ctrl Pts',(-2.92912011817042,-0.776741122275152,
-0.41710939194351));
#17035=CARTESIAN_POINT('Ctrl Pts',(-0.930040753983942,-2.88326355857391,
-0.257959712123399));
#17036=CARTESIAN_POINT('Ctrl Pts',(1.92540990438357,-2.34273649504526,-0.0988100323032949));
#17037=CARTESIAN_POINT('Ctrl Pts',(3.00812651671163,0.358881109808823,0.0603396475168144));
#17038=CARTESIAN_POINT('Ctrl Pts',(1.88996995460182,1.92877590264587,0.166439434063553));
#17039=CARTESIAN_POINT('Ctrl Pts',(1.12236674703444,2.30288577939269,0.219489327336923));
#17040=CARTESIAN_POINT('Ctrl Pts',(0.439445221994093,2.33068358199189,-7.62825));
#17041=CARTESIAN_POINT('Ctrl Pts',(-0.337423613347535,2.47716047848903,
-7.57520010672663));
#17042=CARTESIAN_POINT('Ctrl Pts',(-2.03563801517394,1.92935211656188,-7.4691003201799));
#17043=CARTESIAN_POINT('Ctrl Pts',(-2.72493988491372,-0.675536495339759,
-7.30995064035978));
#17044=CARTESIAN_POINT('Ctrl Pts',(-0.903098151772226,-2.65539425532298,
-7.15080096053969));
#17045=CARTESIAN_POINT('Ctrl Pts',(1.74597935598366,-2.19600765141715,-6.99165128071957));
#17046=CARTESIAN_POINT('Ctrl Pts',(2.79147243493216,0.283269578050224,-6.83250160089946));
#17047=CARTESIAN_POINT('Ctrl Pts',(1.26983859810019,2.50159785776548,-6.67335192107936));
#17048=CARTESIAN_POINT('Ctrl Pts',(-1.4187825692111,2.42038344679719,-6.51420224125925));
#17049=CARTESIAN_POINT('Ctrl Pts',(-2.80328291203716,0.113870415496436,
-6.35505256143915));
#17050=CARTESIAN_POINT('Ctrl Pts',(-1.61049774213476,-2.29725302707627,
-6.19590288161903));
#17051=CARTESIAN_POINT('Ctrl Pts',(1.06282132621106,-2.59645975535387,-6.03675320179892));
#17052=CARTESIAN_POINT('Ctrl Pts',(2.75907820786381,-0.508617350322671,
-5.87760352197883));
#17053=CARTESIAN_POINT('Ctrl Pts',(1.91878831253368,2.04680647949509,-5.7184538421587));
#17054=CARTESIAN_POINT('Ctrl Pts',(-0.685511273604884,2.72052538198363,
-5.55930416233861));
#17055=CARTESIAN_POINT('Ctrl Pts',(-2.65959762385548,0.893154280769607,
-5.40015448251848));
#17056=CARTESIAN_POINT('Ctrl Pts',(-2.18860784384354,-1.75532751220894,
-5.2410048026984));
#17057=CARTESIAN_POINT('Ctrl Pts',(0.294454856588238,-2.79006777499793,
-5.08185512287827));
#17058=CARTESIAN_POINT('Ctrl Pts',(2.50681415110888,-1.25978745570213,-4.92270544305818));
#17059=CARTESIAN_POINT('Ctrl Pts',(2.41455925517875,1.42866531011816,-4.76355576323806));
#17060=CARTESIAN_POINT('Ctrl Pts',(0.102504271982408,2.80368940376361,-4.60440608341796));
#17061=CARTESIAN_POINT('Ctrl Pts',(-2.30378705302599,1.60117036795331,-4.44525640359785));
#17062=CARTESIAN_POINT('Ctrl Pts',(-2.59211535415612,-1.07336817656879,
-4.28610672377774));
#17063=CARTESIAN_POINT('Ctrl Pts',(-0.497409040646124,-2.76111672375383,
-4.12695704395763));
#17064=CARTESIAN_POINT('Ctrl Pts',(2.05458518082845,-1.91046094844367,-3.96780736413752));
#17065=CARTESIAN_POINT('Ctrl Pts',(2.717717602526,0.69655748161016,-3.80865768431742));
#17066=CARTESIAN_POINT('Ctrl Pts',(0.882344250202438,2.66320294535576,-3.64950800449731));
#17067=CARTESIAN_POINT('Ctrl Pts',(-1.76420323128872,2.18146011904347,-3.4903583246772));
#17068=CARTESIAN_POINT('Ctrl Pts',(-2.7888485843108,-0.305785667740972,
-3.33120864485709));
#17069=CARTESIAN_POINT('Ctrl Pts',(-1.24959461996354,-2.51191054810233,
-3.17205896503699));
#17070=CARTESIAN_POINT('Ctrl Pts',(1.43846132446067,-2.40873623914147,-3.01290928521687));
#17071=CARTESIAN_POINT('Ctrl Pts',(2.80408262807151,-0.0911150253769769,
-2.85375960539677));
#17072=CARTESIAN_POINT('Ctrl Pts',(1.59179933506719,2.3102719050862,-2.69460992557666));
#17073=CARTESIAN_POINT('Ctrl Pts',(-1.08388829677707,2.58773397497002,-2.53546024575656));
#17074=CARTESIAN_POINT('Ctrl Pts',(-2.76311442338486,0.486189577250177,
-2.37631056593645));
#17075=CARTESIAN_POINT('Ctrl Pts',(-1.90209953189,-2.0623285922554,-2.21716088611634));
#17076=CARTESIAN_POINT('Ctrl Pts',(0.707590769365126,-2.71486542435539,
-2.05801120629623));
#17077=CARTESIAN_POINT('Ctrl Pts',(2.66676527322589,-0.871519975440165,
-1.89886152647612));
#17078=CARTESIAN_POINT('Ctrl Pts',(2.17427552027739,1.77305104894897,-1.73971184665602));
#17079=CARTESIAN_POINT('Ctrl Pts',(-0.31711023351784,2.787580752663,-1.58056216683591));
#17080=CARTESIAN_POINT('Ctrl Pts',(-2.51696754337392,1.23938636097081,-1.4214124870158));
#17081=CARTESIAN_POINT('Ctrl Pts',(-2.40286970185313,-1.44824363576629,
-1.26226280719569));
#17082=CARTESIAN_POINT('Ctrl Pts',(-0.0797314402530648,-2.80441033824713,
-1.10311312737558));
#17083=CARTESIAN_POINT('Ctrl Pts',(2.31673231987452,-1.58243891335296,-0.94396344755548));
#17084=CARTESIAN_POINT('Ctrl Pts',(2.58328372722621,1.0944611426978,-0.784813767735368));
#17085=CARTESIAN_POINT('Ctrl Pts',(0.47501218998366,2.76493134210758,-0.625664087915265));
#17086=CARTESIAN_POINT('Ctrl Pts',(-2.07013388915155,1.89396559890118,-0.466514408095153));
#17087=CARTESIAN_POINT('Ctrl Pts',(-2.71178477923519,-0.719108356029971,
-0.307364728275049));
#17088=CARTESIAN_POINT('Ctrl Pts',(-0.861033436313082,-2.66933069223121,
-0.148215048454937));
#17089=CARTESIAN_POINT('Ctrl Pts',(1.78254802188085,-2.16890974515266,0.0109346313651662));
#17090=CARTESIAN_POINT('Ctrl Pts',(2.78492904795165,0.332252789872783,0.170084311185276));
#17091=CARTESIAN_POINT('Ctrl Pts',(1.74973765135393,1.78566426924742,0.276184097732015));
#17092=CARTESIAN_POINT('Ctrl Pts',(1.03908919352505,2.13201587949045,0.329233991005384));
#17093=CARTESIAN_POINT('',(1.28892185405323,2.64462557919718,0.));
#17094=CARTESIAN_POINT('Ctrl Pts',(1.28892185405323,2.64462557919718,0.));
#17095=CARTESIAN_POINT('Ctrl Pts',(2.17043456109762,2.21499916944277,-0.0530498932733694));
#17096=CARTESIAN_POINT('Ctrl Pts',(2.8124780076646,1.31356845956184,-0.106099786546739));
#17097=CARTESIAN_POINT('Ctrl Pts',(2.92626843347433,0.345765147202809,-0.159149679820108));
#17098=CARTESIAN_POINT('Ctrl Pts',(3.04005885928406,-0.622038165156221,
-0.212199573093478));
#17099=CARTESIAN_POINT('Ctrl Pts',(2.62559626433654,-1.65621407999334,-0.265249466366847));
#17100=CARTESIAN_POINT('Ctrl Pts',(1.871833457077,-2.27675858681671,-0.318299359640216));
#17101=CARTESIAN_POINT('Ctrl Pts',(1.11807064981746,-2.89730309364007,-0.371349252913585));
#17102=CARTESIAN_POINT('Ctrl Pts',(0.0250076302459046,-3.10421619244968,
-0.424399146186955));
#17103=CARTESIAN_POINT('Ctrl Pts',(-0.904146447325742,-2.80448563577219,
-0.477449039460324));
#17104=CARTESIAN_POINT('Ctrl Pts',(-1.8333005248974,-2.5047550790947,-0.530498932733693));
#17105=CARTESIAN_POINT('Ctrl Pts',(-2.59854566046914,-1.69838086693011,
-0.583548826007063));
#17106=CARTESIAN_POINT('Ctrl Pts',(-2.84851393510817,-0.754969343195062,
-0.636598719280432));
#17107=CARTESIAN_POINT('Ctrl Pts',(-2.91326419433548,-0.510593768702306,
-0.650340440490422));
#17108=CARTESIAN_POINT('Ctrl Pts',(-2.94344011517888,-0.25702318713533,
-0.664082161700412));
#17109=CARTESIAN_POINT('Ctrl Pts',(-2.94115781190101,-0.00289931852541142,
-0.677823882910403));
#17110=CARTESIAN_POINT('Ctrl Pts',(1.38002164928817,-1.93382042716839,-7.7715611723761E-16));
#17111=CARTESIAN_POINT('Ctrl Pts',(1.42812747073086,-1.90764311681531,-7.5694502902296E-16));
#17112=CARTESIAN_POINT('Ctrl Pts',(1.47517679419513,-1.87973274797267,-1.70831917836036E-15));
#17113=CARTESIAN_POINT('Ctrl Pts',(1.52106467934594,-1.85010961136059,-1.94289029309402E-15));
#17114=CARTESIAN_POINT('Ctrl Pts',(1.58950048722442,-1.80593055888783,-2.29363597887594E-15));
#17115=CARTESIAN_POINT('Ctrl Pts',(1.65535434494963,-1.7579446136614,-3.02182188661513E-15));
#17116=CARTESIAN_POINT('Ctrl Pts',(1.71854070901811,-1.70651204529061,-3.60822483003176E-15));
#17117=CARTESIAN_POINT('Ctrl Pts',(1.7555130642401,-1.67641721049804,-3.95134787955118E-15));
#17118=CARTESIAN_POINT('Ctrl Pts',(1.79157183927568,-1.64514134213701,-1.07060037084947E-15));
#17119=CARTESIAN_POINT('Ctrl Pts',(1.82669682228498,-1.61274915084688,-1.16573417585641E-15));
#17120=CARTESIAN_POINT('Ctrl Pts',(1.841722159954,-1.59889281355429,-1.20642935693563E-15));
#17121=CARTESIAN_POINT('Ctrl Pts',(1.85657659510814,-1.58483214201628,-3.58134186129285E-15));
#17122=CARTESIAN_POINT('Ctrl Pts',(1.87125839132482,-1.57057192863285,-3.77475828372553E-15));
#17123=CARTESIAN_POINT('Ctrl Pts',(1.88495537365188,-1.5572682505399,-3.95520087267901E-15));
#17124=CARTESIAN_POINT('Ctrl Pts',(1.89850308492679,-1.54378970611349,-1.28299784462317E-15));
#17125=CARTESIAN_POINT('Ctrl Pts',(1.91188526750315,-1.53015568567424,-1.33226762955019E-15));
#17126=CARTESIAN_POINT('Ctrl Pts',(1.97177620973344,-1.46913766220646,-1.5527708117424E-15));
#17127=CARTESIAN_POINT('Ctrl Pts',(2.02842345123512,-1.40494307633604,-3.57723878703623E-15));
#17128=CARTESIAN_POINT('Ctrl Pts',(2.0817308935379,-1.33796367996907,-3.44169137633799E-15));
#17129=CARTESIAN_POINT('Ctrl Pts',(2.127945639128,-1.2798960700977,-3.32417890846838E-15));
#17130=CARTESIAN_POINT('Ctrl Pts',(2.17165011443041,-1.21973426244966,-1.81697204400015E-15));
#17131=CARTESIAN_POINT('Ctrl Pts',(2.21276616256005,-1.15770575782311,-1.83186799063151E-15));
#17132=CARTESIAN_POINT('Ctrl Pts',(2.2325537470201,-1.12785380633305,-1.83903684112879E-15));
#17133=CARTESIAN_POINT('Ctrl Pts',(2.25174157820912,-1.09756915706639,-2.28535431450448E-15));
#17134=CARTESIAN_POINT('Ctrl Pts',(2.27031947398645,-1.06687542421666,-2.58126853225349E-15));
#17135=CARTESIAN_POINT('Ctrl Pts',(2.28192871071775,-1.04769505981529,-2.76618388796334E-15));
#17136=CARTESIAN_POINT('Ctrl Pts',(2.29330289136903,-1.02834915196317,6.32263275798518E-17));
#17137=CARTESIAN_POINT('Ctrl Pts',(2.30442183390172,-1.00887472850267,5.55111512312578E-17));
#17138=CARTESIAN_POINT('Ctrl Pts',(2.34839407475996,-0.931858947868614,
2.49998331210308E-17));
#17139=CARTESIAN_POINT('Ctrl Pts',(2.38842162089745,-0.8527674310775,-3.06551327022485E-15));
#17140=CARTESIAN_POINT('Ctrl Pts',(2.42440442503016,-0.771996655564967,
-2.72004641033163E-15));
#17141=CARTESIAN_POINT('Ctrl Pts',(2.46243949056497,-0.686619158897789,
-2.35487601928374E-15));
#17142=CARTESIAN_POINT('Ctrl Pts',(2.49595626081657,-0.599364864549967,
6.80623617719379E-16));
#17143=CARTESIAN_POINT('Ctrl Pts',(2.52479802771902,-0.510654497756694,
1.27675647831893E-15));
#17144=CARTESIAN_POINT('Ctrl Pts',(2.55242599313135,-0.425677493616475,
1.84780117573675E-15));
#17145=CARTESIAN_POINT('Ctrl Pts',(2.57576446764424,-0.33936327234262,2.22743437905015E-16));
#17146=CARTESIAN_POINT('Ctrl Pts',(2.59463283383731,-0.252052712602013,
2.77555756156289E-16));
#17147=CARTESIAN_POINT('Ctrl Pts',(2.60106539892371,-0.222286973877501,
2.96242260386698E-16));
#17148=CARTESIAN_POINT('Ctrl Pts',(2.60697802607669,-0.192405253045208,
-1.3763582714056E-15));
#17149=CARTESIAN_POINT('Ctrl Pts',(2.61236225462784,-0.162420585421049,
-1.4432899320127E-15));
#17150=CARTESIAN_POINT('Ctrl Pts',(2.61541762236764,-0.145405299892759,
-1.48127138741476E-15));
#17151=CARTESIAN_POINT('Ctrl Pts',(2.61830282357874,-0.128356860267427,
-2.88095861055776E-15));
#17152=CARTESIAN_POINT('Ctrl Pts',(2.62101620860007,-0.111277626913365,
-2.99760216648792E-15));
#17153=CARTESIAN_POINT('Ctrl Pts',(2.62313739988994,-0.0979259201914906,
-3.08878837593249E-15));
#17154=CARTESIAN_POINT('Ctrl Pts',(2.62515315328059,-0.0845577480124575,
-1.4025265292375E-15));
#17155=CARTESIAN_POINT('Ctrl Pts',(2.62706136230965,-0.0711852941876254,
-1.36002320516582E-15));
#17156=CARTESIAN_POINT('Ctrl Pts',(2.64014127982351,0.0204768823995774,
-1.06868197134027E-15));
#17157=CARTESIAN_POINT('Ctrl Pts',(2.64819506516295,0.112482484208663,-2.30351243816908E-15));
#17158=CARTESIAN_POINT('Ctrl Pts',(2.65108741954648,0.204436910520549,-2.13717932240343E-15));
#17159=CARTESIAN_POINT('Ctrl Pts',(2.6522300189544,0.240762705747386,-2.07147087371765E-15));
#17160=CARTESIAN_POINT('Ctrl Pts',(2.6525666724142,0.277080849976937,1.38410269878359E-15));
#17161=CARTESIAN_POINT('Ctrl Pts',(2.65208709596217,0.313368136238073,1.36002320516582E-15));
#17162=CARTESIAN_POINT('Ctrl Pts',(2.65091611137812,0.401971012023442,1.30322121910574E-15));
#17163=CARTESIAN_POINT('Ctrl Pts',(2.64488261707637,0.490389342189787,3.16280801020804E-17));
#17164=CARTESIAN_POINT('Ctrl Pts',(2.6342319072788,0.578361332654982,-1.38777878078145E-16));
#17165=CARTESIAN_POINT('Ctrl Pts',(2.62336505681307,0.668118586746737,-3.12641977392605E-16));
#17166=CARTESIAN_POINT('Ctrl Pts',(2.60769159491865,0.757411929633459,-1.18972610440493E-15));
#17167=CARTESIAN_POINT('Ctrl Pts',(2.58741809056973,0.845967129974637,-1.22124532708767E-15));
#17168=CARTESIAN_POINT('Ctrl Pts',(2.58188375720388,0.870141243711141,-1.22984955666519E-15));
#17169=CARTESIAN_POINT('Ctrl Pts',(2.57600632881146,0.894260336658512,-2.52103891604412E-15));
#17170=CARTESIAN_POINT('Ctrl Pts',(2.56978934466171,0.918318763783367,-2.65065747129256E-15));
#17171=CARTESIAN_POINT('Ctrl Pts',(2.56617655991,0.932299484430771,-2.72598079988109E-15));
#17172=CARTESIAN_POINT('Ctrl Pts',(2.56245121029721,0.946251475332682,-1.21864460931396E-15));
#17173=CARTESIAN_POINT('Ctrl Pts',(2.55861555514304,0.960169583265971,-1.17961196366423E-15));
#17174=CARTESIAN_POINT('Ctrl Pts',(2.53400743126124,1.0494629400605,-9.29193158799269E-16));
#17175=CARTESIAN_POINT('Ctrl Pts',(2.5048497143222,1.13741458886572,-5.45198539607864E-16));
#17176=CARTESIAN_POINT('Ctrl Pts',(2.47143088982083,1.22374100902459,-3.33066907387547E-16));
#17177=CARTESIAN_POINT('Ctrl Pts',(2.43737301009748,1.31171821584098,-1.16878764223515E-16));
#17178=CARTESIAN_POINT('Ctrl Pts',(2.39888933062496,1.39800823053115,9.879708656971E-16));
#17179=CARTESIAN_POINT('Ctrl Pts',(2.35622978660644,1.48231381194112,1.29063426612674E-15));
#17180=CARTESIAN_POINT('Ctrl Pts',(2.31321870904863,1.56731410868612,1.59579174704448E-15));
#17181=CARTESIAN_POINT('Ctrl Pts',(2.26596236943433,1.65029800809477,-2.42731618613007E-15));
#17182=CARTESIAN_POINT('Ctrl Pts',(2.21466476470311,1.73095108378988,-2.63677968348475E-15));
#17183=CARTESIAN_POINT('Ctrl Pts',(2.18386460320696,1.77937688787153,-2.76254597569037E-15));
#17184=CARTESIAN_POINT('Ctrl Pts',(2.15160656205411,1.82696217117237,-2.40998514952242E-15));
#17185=CARTESIAN_POINT('Ctrl Pts',(2.11792656714594,1.87363515402618,-2.49106291150269E-15));
#17186=CARTESIAN_POINT('Ctrl Pts',(2.10877443900116,1.88631796829447,-2.51309480519384E-15));
#17187=CARTESIAN_POINT('Ctrl Pts',(2.09951639417844,1.89893445563434,-2.77486678097692E-15));
#17188=CARTESIAN_POINT('Ctrl Pts',(2.09016420919922,1.91146858929654,-2.69922972861991E-15));
#17189=CARTESIAN_POINT('Ctrl Pts',(2.03135556865992,1.99028603812276,-2.22360694812491E-15));
#17190=CARTESIAN_POINT('Ctrl Pts',(1.96873479008562,2.06598007149761,-4.57292501631552E-16));
#17191=CARTESIAN_POINT('Ctrl Pts',(1.90257280213557,2.13824089870506,-6.38378239159465E-16));
#17192=CARTESIAN_POINT('Ctrl Pts',(1.83625579712803,2.2106710325061,-8.19888259255879E-16));
#17193=CARTESIAN_POINT('Ctrl Pts',(1.76638056903207,2.27965275545374,1.58499855722304E-15));
#17194=CARTESIAN_POINT('Ctrl Pts',(1.69316997818223,2.3448583260052,1.31492039479042E-15));
#17195=CARTESIAN_POINT('Ctrl Pts',(1.62138713583198,2.4087922614771,1.05010928029049E-15));
#17196=CARTESIAN_POINT('Ctrl Pts',(1.54639722394925,2.46909666244371,4.27974250822394E-16));
#17197=CARTESIAN_POINT('Ctrl Pts',(1.46836948021005,2.52543520618547,1.07552855510562E-15));
#17198=CARTESIAN_POINT('Ctrl Pts',(1.4102223701464,2.56741929218862,1.55809295590647E-15));
#17199=CARTESIAN_POINT('Ctrl Pts',(1.35038736882638,2.60720050088858,6.55137100424993E-17));
#17200=CARTESIAN_POINT('Ctrl Pts',(1.28892185405323,2.64462557919718,0.));
#17201=CARTESIAN_POINT('Ctrl Pts',(0.439445221994093,2.33068358199189,-7.62825));
#17202=CARTESIAN_POINT('Ctrl Pts',(-0.337423613347535,2.47716047848903,
-7.57520010672663));
#17203=CARTESIAN_POINT('Ctrl Pts',(-1.82948700838562,1.99585210927004,-7.48198007069497));
#17204=CARTESIAN_POINT('Ctrl Pts',(-2.3653507640067,0.596861175155798,-7.38876003466331));
#17205=CARTESIAN_POINT('Ctrl Pts',(-2.37144645257593,-0.00213225654898062,
-7.34858989190502));
#17206=CARTESIAN_POINT('Origin',(0.,0.,-8.));
#17207=CARTESIAN_POINT('',(-1.28892185405322,2.64462557919718,0.));
#17208=CARTESIAN_POINT('Ctrl Pts',(-2.94163492837973,-0.00273205723265913,
-0.822176117089598));
#17209=CARTESIAN_POINT('Ctrl Pts',(-2.94382357462719,-0.242779219769019,
-0.809190456057937));
#17210=CARTESIAN_POINT('Ctrl Pts',(-2.91690973953269,-0.48233937851609,
-0.796204795026276));
#17211=CARTESIAN_POINT('Ctrl Pts',(-2.85900606151163,-0.714154570807424,
-0.783219133994616));
#17212=CARTESIAN_POINT('Ctrl Pts',(-2.62279267049859,-1.65982597771804,
-0.730245175661282));
#17213=CARTESIAN_POINT('Ctrl Pts',(-1.87085675264489,-2.47660826181784,
-0.677271217327949));
#17214=CARTESIAN_POINT('Ctrl Pts',(-0.947905463978179,-2.79019041180322,
-0.624297258994615));
#17215=CARTESIAN_POINT('Ctrl Pts',(-0.0249541753114783,-3.1037725617886,
-0.571323300661282));
#17216=CARTESIAN_POINT('Ctrl Pts',(1.06901248416821,-2.91415457765955,-0.518349342327949));
#17217=CARTESIAN_POINT('Ctrl Pts',(1.832390730231,-2.30797131654626,-0.465375383994615));
#17218=CARTESIAN_POINT('Ctrl Pts',(2.59576897629379,-1.70178805543296,-0.412401425661282));
#17219=CARTESIAN_POINT('Ctrl Pts',(3.02855880893968,-0.679039517335424,
-0.359427467327948));
#17220=CARTESIAN_POINT('Ctrl Pts',(2.93245036408289,0.290806479998895,-0.306453508994615));
#17221=CARTESIAN_POINT('Ctrl Pts',(2.83634191922609,1.26065247733321,-0.253479550661282));
#17222=CARTESIAN_POINT('Ctrl Pts',(2.21133519686661,2.17759593390431,-0.200505592327948));
#17223=CARTESIAN_POINT('Ctrl Pts',(1.34376500468284,2.62235303498606,-0.147531633994614));
#17224=CARTESIAN_POINT('Ctrl Pts',(0.538375261717025,3.03523352644325,-0.0983544226630757));
#17225=CARTESIAN_POINT('Ctrl Pts',(-0.476053973012966,3.04118713875837,
-0.0491772113315374));
#17226=CARTESIAN_POINT('Ctrl Pts',(-1.29202279186848,2.64852742499071,1.17961196366423E-15));
#17227=CARTESIAN_POINT('Origin',(0.,0.,0.));
#17228=CARTESIAN_POINT('Origin',(1.15470053837925,2.,28.));
#17229=CARTESIAN_POINT('',(1.15470053837925,2.,28.));
#17230=CARTESIAN_POINT('',(2.3094010767585,0.,28.));
#17231=CARTESIAN_POINT('',(1.44337567297406,1.5,28.));
#17232=CARTESIAN_POINT('',(1.15470053837925,2.,25.));
#17233=CARTESIAN_POINT('',(1.15470053837925,2.,28.));
#17234=CARTESIAN_POINT('',(2.3094010767585,0.,25.));
#17235=CARTESIAN_POINT('',(2.3094010767585,0.,25.));
#17236=CARTESIAN_POINT('',(2.3094010767585,0.,28.));
#17237=CARTESIAN_POINT('Origin',(-1.15470053837925,2.,28.));
#17238=CARTESIAN_POINT('',(-1.15470053837925,2.,28.));
#17239=CARTESIAN_POINT('',(-0.577350269189626,2.,28.));
#17240=CARTESIAN_POINT('',(-1.15470053837925,2.,25.));
#17241=CARTESIAN_POINT('',(-1.15470053837925,2.,28.));
#17242=CARTESIAN_POINT('',(1.15470053837925,2.,25.));
#17243=CARTESIAN_POINT('Origin',(-2.3094010767585,2.77555756156289E-16,
28.));
#17244=CARTESIAN_POINT('',(-2.3094010767585,2.82820063659975E-16,28.));
#17245=CARTESIAN_POINT('',(-2.02072594216369,0.5,28.));
#17246=CARTESIAN_POINT('',(-2.3094010767585,2.77555756156289E-16,25.));
#17247=CARTESIAN_POINT('',(-2.3094010767585,2.82820063659975E-16,28.));
#17248=CARTESIAN_POINT('',(-1.15470053837925,2.,25.));
#17249=CARTESIAN_POINT('Origin',(-1.15470053837925,-2.,28.));
#17250=CARTESIAN_POINT('',(-1.15470053837925,-2.,28.));
#17251=CARTESIAN_POINT('',(-1.44337567297407,-1.5,28.));
#17252=CARTESIAN_POINT('',(-1.15470053837925,-2.,25.));
#17253=CARTESIAN_POINT('',(-1.15470053837925,-2.,28.));
#17254=CARTESIAN_POINT('',(-2.3094010767585,2.82820063659975E-16,25.));
#17255=CARTESIAN_POINT('Origin',(1.15470053837925,-2.,28.));
#17256=CARTESIAN_POINT('',(1.15470053837925,-2.,28.));
#17257=CARTESIAN_POINT('',(0.577350269189626,-2.,28.));
#17258=CARTESIAN_POINT('',(1.15470053837925,-2.,25.));
#17259=CARTESIAN_POINT('',(1.15470053837925,-2.,28.));
#17260=CARTESIAN_POINT('',(-1.15470053837925,-2.,25.));
#17261=CARTESIAN_POINT('Origin',(2.3094010767585,0.,28.));
#17262=CARTESIAN_POINT('',(2.02072594216369,-0.5,28.));
#17263=CARTESIAN_POINT('',(1.15470053837925,-2.,25.));
#17264=CARTESIAN_POINT('Origin',(0.,0.,25.));
#17265=CARTESIAN_POINT('Ctrl Pts',(2.34668236863854,0.343918483395443,-7.62825));
#17266=CARTESIAN_POINT('Ctrl Pts',(2.23221075339669,1.12500043789087,-7.57527604166667));
#17267=CARTESIAN_POINT('Ctrl Pts',(1.16389372259185,2.55030135594479,-7.469328125));
#17268=CARTESIAN_POINT('Ctrl Pts',(-1.5190222941925,2.35934508271871,-7.31040625));
#17269=CARTESIAN_POINT('Ctrl Pts',(-2.80340787029919,0.000687648512017017,
-7.15148437500001));
#17270=CARTESIAN_POINT('Ctrl Pts',(-1.52008573002868,-2.35640251272322,
-6.99256249999999));
#17271=CARTESIAN_POINT('Ctrl Pts',(1.15851212495977,-2.55397203032575,-6.833640625));
#17272=CARTESIAN_POINT('Ctrl Pts',(2.77407199314419,-0.40912796830676,-6.67471874999999));
#17273=CARTESIAN_POINT('Ctrl Pts',(1.8463937974617,2.11054799657883,-6.515796875));
#17274=CARTESIAN_POINT('Ctrl Pts',(-0.774509592452447,2.6951571659338,-6.356875));
#17275=CARTESIAN_POINT('Ctrl Pts',(-2.68513189196673,0.808405636158886,
-6.197953125));
#17276=CARTESIAN_POINT('Ctrl Pts',(-2.13372739995655,-1.81955463387985,
-6.03903125));
#17277=CARTESIAN_POINT('Ctrl Pts',(0.374189682251391,-2.77913011091259,
-5.88010937499999));
#17278=CARTESIAN_POINT('Ctrl Pts',(2.53898480026785,-1.19042008723587,-5.7211875));
#17279=CARTESIAN_POINT('Ctrl Pts',(2.37571150505774,1.48981793161623,-5.562265625));
#17280=CARTESIAN_POINT('Ctrl Pts',(0.0340680162793398,2.80399746681091,
-5.40334375));
#17281=CARTESIAN_POINT('Ctrl Pts',(-2.33881132397979,1.54710018774848,-5.244421875));
#17282=CARTESIAN_POINT('Ctrl Pts',(-2.56716079869307,-1.12838190825516,
-5.0855));
#17283=CARTESIAN_POINT('Ctrl Pts',(-0.441597707549828,-2.76921495982712,
-4.926578125));
#17284=CARTESIAN_POINT('Ctrl Pts',(2.0888801521554,-1.870865869044,-4.76765625));
#17285=CARTESIAN_POINT('Ctrl Pts',(2.70399705609256,0.742939933921091,-4.608734375));
#17286=CARTESIAN_POINT('Ctrl Pts',(0.839732362462355,2.67552038173531,-4.4498125));
#17287=CARTESIAN_POINT('Ctrl Pts',(-1.79450978671873,2.15483045727933,-4.290890625));
#17288=CARTESIAN_POINT('Ctrl Pts',(-2.78330845646984,-0.341692515414928,
-4.13196875));
#17289=CARTESIAN_POINT('Ctrl Pts',(-1.22000243857572,-2.52490668674665,
-3.973046875));
#17290=CARTESIAN_POINT('Ctrl Pts',(1.46196288604333,-2.39295303517309,-3.814125));
#17291=CARTESIAN_POINT('Ctrl Pts',(2.80340761681022,-0.0668241043267523,
-3.655203125));
#17292=CARTESIAN_POINT('Ctrl Pts',(1.57431810519612,2.32057799752537,-3.49628125));
#17293=CARTESIAN_POINT('Ctrl Pts',(-1.09831409983361,2.58016778763604,-3.337359375));
#17294=CARTESIAN_POINT('Ctrl Pts',(-2.76386693296932,0.47391911808494,-3.1784375));
#17295=CARTESIAN_POINT('Ctrl Pts',(-1.89514163556503,-2.06688122685359,
-3.019515625));
#17296=CARTESIAN_POINT('Ctrl Pts',(0.71129970966804,-2.71249186414424,-2.86059375));
#17297=CARTESIAN_POINT('Ctrl Pts',(2.66552760696098,-0.870932032693957,
-2.701671875));
#17298=CARTESIAN_POINT('Ctrl Pts',(2.17564778740008,1.76921366782114,-2.54275));
#17299=CARTESIAN_POINT('Ctrl Pts',(-0.309153032213342,2.78710993733308,
-2.383828125));
#17300=CARTESIAN_POINT('Ctrl Pts',(-2.51048180952901,1.24941726722468,-2.22490625));
#17301=CARTESIAN_POINT('Ctrl Pts',(-2.40986887600225,-1.43390886220311,
-2.065984375));
#17302=CARTESIAN_POINT('Ctrl Pts',(-0.0995709890729291,-2.80243276783242,
-1.9070625));
#17303=CARTESIAN_POINT('Ctrl Pts',(2.30202865838936,-1.60132637136797,-1.748140625));
#17304=CARTESIAN_POINT('Ctrl Pts',(2.59282079624265,1.06810673697464,-1.58921875));
#17305=CARTESIAN_POINT('Ctrl Pts',(0.506179573027947,2.75812167782342,-1.430296875));
#17306=CARTESIAN_POINT('Ctrl Pts',(-2.04460746115808,1.91919712058503,-1.271375));
#17307=CARTESIAN_POINT('Ctrl Pts',(-2.72060249130678,-0.679635921257337,
-1.112453125));
#17308=CARTESIAN_POINT('Ctrl Pts',(-0.902039595484687,-2.65503026080224,
-0.953531249999998));
#17309=CARTESIAN_POINT('Ctrl Pts',(1.74372732289156,-2.19643768378856,-0.794609375000001));
#17310=CARTESIAN_POINT('Ctrl Pts',(2.79043291661474,0.277087651255129,-0.635687499999998));
#17311=CARTESIAN_POINT('Ctrl Pts',(1.2788492724039,2.49472256946297,-0.476765624999999));
#17312=CARTESIAN_POINT('Ctrl Pts',(-1.4060176679778,2.42838470324144,-0.317843749999998));
#17313=CARTESIAN_POINT('Ctrl Pts',(-2.80039548414902,0.128338365192599,
-0.158921874999999));
#17314=CARTESIAN_POINT('Ctrl Pts',(-2.01976953076572,-1.47272600147648,
-0.0529739583333322));
#17315=CARTESIAN_POINT('Ctrl Pts',(-1.37702479013101,-1.93106208855766,
1.11022302462516E-15));
#17316=CARTESIAN_POINT('Ctrl Pts',(2.53475666268529,0.371481747533205,-7.51850533633154));
#17317=CARTESIAN_POINT('Ctrl Pts',(2.41111074737083,1.2151633274179,-7.4655313779982));
#17318=CARTESIAN_POINT('Ctrl Pts',(1.25717370506724,2.75469464475791,-7.35958346133153));
#17319=CARTESIAN_POINT('Ctrl Pts',(-1.64076397062878,2.54843422693997,-7.20066158633155));
#17320=CARTESIAN_POINT('Ctrl Pts',(-3.02808631983197,0.000742759936635549,
-7.04173971133153));
#17321=CARTESIAN_POINT('Ctrl Pts',(-1.6419126352743,-2.54525582537989,-6.88281783633154));
#17322=CARTESIAN_POINT('Ctrl Pts',(1.25136080058723,-2.75865950445431,-6.72389596133153));
#17323=CARTESIAN_POINT('Ctrl Pts',(2.99639932585779,-0.441917430929573,
-6.56497408633154));
#17324=CARTESIAN_POINT('Ctrl Pts',(1.99437258429316,2.27969735816824,-6.40605221133153));
#17325=CARTESIAN_POINT('Ctrl Pts',(-0.836582477466464,2.91115988880001,
-6.24713033633154));
#17326=CARTESIAN_POINT('Ctrl Pts',(-2.90033114166196,0.873195111443611,
-6.08820846133153));
#17327=CARTESIAN_POINT('Ctrl Pts',(-2.30473446925493,-1.96538240240098,
-5.92928658633154));
#17328=CARTESIAN_POINT('Ctrl Pts',(0.404179024341101,-3.00186282525825,
-5.77036471133153));
#17329=CARTESIAN_POINT('Ctrl Pts',(2.74247112644792,-1.28582601882594,-5.61144283633154));
#17330=CARTESIAN_POINT('Ctrl Pts',(2.56611233226117,1.60921903143761,-5.45252096133153));
#17331=CARTESIAN_POINT('Ctrl Pts',(0.0367983892505396,3.02872316941433,
-5.29359908633154));
#17332=CARTESIAN_POINT('Ctrl Pts',(-2.52625479504538,1.67109216021095,-5.13467721133154));
#17333=CARTESIAN_POINT('Ctrl Pts',(-2.77290528349047,-1.21881580491128,
-4.97575533633154));
#17334=CARTESIAN_POINT('Ctrl Pts',(-0.476989449615156,-2.99115302677367,
-4.81683346133153));
#17335=CARTESIAN_POINT('Ctrl Pts',(2.25629294956471,-2.02080596416678,-4.65791158633154));
#17336=CARTESIAN_POINT('Ctrl Pts',(2.9207082498295,0.802482676244758,-4.49898971133153));
#17337=CARTESIAN_POINT('Ctrl Pts',(0.907032510692453,2.88994931925466,-4.34006783633155));
#17338=CARTESIAN_POINT('Ctrl Pts',(-1.93833034198753,2.32752882603146,-4.18114596133153));
#17339=CARTESIAN_POINT('Ctrl Pts',(-3.00637604331527,-0.369077379884247,
-4.02222408633155));
#17340=CARTESIAN_POINT('Ctrl Pts',(-1.31777924059923,-2.72726472590441,
-3.86330221133153));
#17341=CARTESIAN_POINT('Ctrl Pts',(1.57913154993654,-2.58473568066095,-3.70438033633154));
#17342=CARTESIAN_POINT('Ctrl Pts',(3.02808604602719,-0.0721797060965247,
-3.54545846133154));
#17343=CARTESIAN_POINT('Ctrl Pts',(1.7004914511064,2.50656016302747,-3.38653658633154));
#17344=CARTESIAN_POINT('Ctrl Pts',(-1.18633821921523,2.78695471443404,-3.22761471133154));
#17345=CARTESIAN_POINT('Ctrl Pts',(-2.98537638358957,0.511901251824159,
-3.06869283633154));
#17346=CARTESIAN_POINT('Ctrl Pts',(-2.04702730615721,-2.23253092568543,
-2.90977096133154));
#17347=CARTESIAN_POINT('Ctrl Pts',(0.768306653828565,-2.92988387222945,
-2.75084908633154));
#17348=CARTESIAN_POINT('Ctrl Pts',(2.87915567594935,-0.940732670991103,
-2.59192721133154));
#17349=CARTESIAN_POINT('Ctrl Pts',(2.35001455606807,1.91100687172472,-2.43300533633154));
#17350=CARTESIAN_POINT('Ctrl Pts',(-0.333930027627364,3.01048219294801,
-2.27408346133154));
#17351=CARTESIAN_POINT('Ctrl Pts',(-2.71168377037141,1.34955151361587,-2.11516158633154));
#17352=CARTESIAN_POINT('Ctrl Pts',(-2.60300723748502,-1.54882914310277,
-1.95623971133154));
#17353=CARTESIAN_POINT('Ctrl Pts',(-0.10755108204491,-3.02703306801251,
-1.79731783633154));
#17354=CARTESIAN_POINT('Ctrl Pts',(2.48652419156761,-1.72966428827498,-1.63839596133154));
#17355=CARTESIAN_POINT('Ctrl Pts',(2.80062179537232,1.15370989452494,-1.47947408633154));
#17356=CARTESIAN_POINT('Ctrl Pts',(0.546747213169786,2.97917067635177,-1.32055221133154));
#17357=CARTESIAN_POINT('Ctrl Pts',(-2.20847203439519,2.07301071223869,-1.16163033633154));
#17358=CARTESIAN_POINT('Ctrl Pts',(-2.93864452365529,-0.734105178710968,
-1.00270846133154));
#17359=CARTESIAN_POINT('Ctrl Pts',(-0.974333341920184,-2.86781702250738,
-0.843786586331539));
#17360=CARTESIAN_POINT('Ctrl Pts',(1.88347792981034,-2.37247065370254,-0.684864711331538));
#17361=CARTESIAN_POINT('Ctrl Pts',(3.01407149160502,0.299294774424126,-0.525942836331538));
#17362=CARTESIAN_POINT('Ctrl Pts',(1.38134233977164,2.69466150980045,-0.367020961331536));
#17363=CARTESIAN_POINT('Ctrl Pts',(-1.51870261582422,2.62300701124516,-0.208099086331538));
#17364=CARTESIAN_POINT('Ctrl Pts',(-3.02483250671829,0.138624012605004,
-0.0491772113315371));
#17365=CARTESIAN_POINT('Ctrl Pts',(-2.18164347404518,-1.5907572726675,0.0567707053351293));
#17366=CARTESIAN_POINT('Ctrl Pts',(-1.48738611075533,-2.08582659521589,
0.109744663668463));
#17367=CARTESIAN_POINT('Ctrl Pts',(2.72283095673204,0.399045011670968,-7.40876067266308));
#17368=CARTESIAN_POINT('Ctrl Pts',(2.59001074134497,1.30532621694494,-7.35578671432974));
#17369=CARTESIAN_POINT('Ctrl Pts',(1.35045368754263,2.95908793357102,-7.24983879766308));
#17370=CARTESIAN_POINT('Ctrl Pts',(-1.76250564706505,2.73752337116124,-7.09091692266307));
#17371=CARTESIAN_POINT('Ctrl Pts',(-3.25276476936475,0.000797871361256092,
-6.93199504766308));
#17372=CARTESIAN_POINT('Ctrl Pts',(-1.76373954051992,-2.73410913803656,
-6.77307317266308));
#17373=CARTESIAN_POINT('Ctrl Pts',(1.34420947621469,-2.96334697858288,-6.61415129766307));
#17374=CARTESIAN_POINT('Ctrl Pts',(3.21872665857139,-0.474706893552386,
-6.45522942266308));
#17375=CARTESIAN_POINT('Ctrl Pts',(2.14235137112462,2.44884671975765,-6.29630754766308));
#17376=CARTESIAN_POINT('Ctrl Pts',(-0.898655362480478,3.12716261166621,
-6.13738567266308));
#17377=CARTESIAN_POINT('Ctrl Pts',(-3.11553039135719,0.937984586728336,
-5.97846379766308));
#17378=CARTESIAN_POINT('Ctrl Pts',(-2.4757415385533,-2.11121017092211,-5.81954192266308));
#17379=CARTESIAN_POINT('Ctrl Pts',(0.434168366430812,-3.2245955396039,-5.66062004766308));
#17380=CARTESIAN_POINT('Ctrl Pts',(2.94595745262798,-1.38123195041602,-5.50169817266308));
#17381=CARTESIAN_POINT('Ctrl Pts',(2.75651315946459,1.728620131259,-5.34277629766308));
#17382=CARTESIAN_POINT('Ctrl Pts',(0.0395287622217419,3.25344887201774,
-5.18385442266308));
#17383=CARTESIAN_POINT('Ctrl Pts',(-2.71369826611098,1.79508413267342,-5.02493254766308));
#17384=CARTESIAN_POINT('Ctrl Pts',(-2.97864976828788,-1.3092497015674,-4.86601067266307));
#17385=CARTESIAN_POINT('Ctrl Pts',(-0.512381191680485,-3.21309109372021,
-4.70708879766308));
#17386=CARTESIAN_POINT('Ctrl Pts',(2.42370574697401,-2.17074605928956,-4.54816692266308));
#17387=CARTESIAN_POINT('Ctrl Pts',(3.13741944356645,0.862025418568423,-4.38924504766307));
#17388=CARTESIAN_POINT('Ctrl Pts',(0.974332658922546,3.104378256774,-4.23032317266308));
#17389=CARTESIAN_POINT('Ctrl Pts',(-2.08215089725633,2.50022719478358,-4.07140129766307));
#17390=CARTESIAN_POINT('Ctrl Pts',(-3.2294436301607,-0.396462244353565,
-3.91247942266308));
#17391=CARTESIAN_POINT('Ctrl Pts',(-1.41555604262275,-2.92962276506217,
-3.75355754766307));
#17392=CARTESIAN_POINT('Ctrl Pts',(1.69630021382975,-2.7765183261488,-3.59463567266308));
#17393=CARTESIAN_POINT('Ctrl Pts',(3.25276447524416,-0.0775353078662964,
-3.43571379766308));
#17394=CARTESIAN_POINT('Ctrl Pts',(1.82666479701668,2.69254232852956,-3.27679192266308));
#17395=CARTESIAN_POINT('Ctrl Pts',(-1.27436233859685,2.99374164123204,-3.11787004766308));
#17396=CARTESIAN_POINT('Ctrl Pts',(-3.20688583420982,0.549883385563377,
-2.95894817266308));
#17397=CARTESIAN_POINT('Ctrl Pts',(-2.19891297674939,-2.39818062451726,
-2.80002629766308));
#17398=CARTESIAN_POINT('Ctrl Pts',(0.825313597989087,-3.14727588031465,
-2.64110442266308));
#17399=CARTESIAN_POINT('Ctrl Pts',(3.09278374493772,-1.01053330928825,-2.48218254766308));
#17400=CARTESIAN_POINT('Ctrl Pts',(2.52438132473606,2.05280007562831,-2.32326067266307));
#17401=CARTESIAN_POINT('Ctrl Pts',(-0.358707023041385,3.23385444856295,
-2.16433879766308));
#17402=CARTESIAN_POINT('Ctrl Pts',(-2.91288573121381,1.44968576000706,-2.00541692266308));
#17403=CARTESIAN_POINT('Ctrl Pts',(-2.79614559896779,-1.66374942400242,
-1.84649504766308));
#17404=CARTESIAN_POINT('Ctrl Pts',(-0.11553117501689,-3.25163336819261,
-1.68757317266307));
#17405=CARTESIAN_POINT('Ctrl Pts',(2.67101972474585,-1.858002205182,-1.52865129766308));
#17406=CARTESIAN_POINT('Ctrl Pts',(3.00842279450199,1.23931305207524,-1.36972942266307));
#17407=CARTESIAN_POINT('Ctrl Pts',(0.587314853311628,3.20021967488011,-1.21080754766308));
#17408=CARTESIAN_POINT('Ctrl Pts',(-2.37233660763231,2.22682430389234,-1.05188567266308));
#17409=CARTESIAN_POINT('Ctrl Pts',(-3.15668655600379,-0.7885744361646,-0.892963797663079));
#17410=CARTESIAN_POINT('Ctrl Pts',(-1.04662708835568,-3.08060378421251,
-0.734041922663075));
#17411=CARTESIAN_POINT('Ctrl Pts',(2.02322853672912,-2.54850362361652,-0.575120047663078));
#17412=CARTESIAN_POINT('Ctrl Pts',(3.23771006659529,0.321501897593122,-0.416198172663076));
#17413=CARTESIAN_POINT('Ctrl Pts',(1.48383540713939,2.89460045013793,-0.257276297663075));
#17414=CARTESIAN_POINT('Ctrl Pts',(-1.63138756367065,2.81762931924888,-0.0983544226630758));
#17415=CARTESIAN_POINT('Ctrl Pts',(-3.24926952928756,0.148909660017409,
0.0605674523369241));
#17416=CARTESIAN_POINT('Ctrl Pts',(-2.34351741732464,-1.70878854385852,
0.166515369003591));
#17417=CARTESIAN_POINT('Ctrl Pts',(-1.59774743137966,-2.24059110187412,
0.219489327336924));
#17418=CARTESIAN_POINT('Ctrl Pts',(2.91090525077879,0.426608275808731,-7.29901600899462));
#17419=CARTESIAN_POINT('Ctrl Pts',(2.7689107353191,1.39548910647197,-7.24604205066128));
#17420=CARTESIAN_POINT('Ctrl Pts',(1.44373367001803,3.16348122238413,-7.14009413399461));
#17421=CARTESIAN_POINT('Ctrl Pts',(-1.88424732350133,2.9266125153825,-6.98117225899462));
#17422=CARTESIAN_POINT('Ctrl Pts',(-3.47744321889753,0.000852982785874625,
-6.82225038399461));
#17423=CARTESIAN_POINT('Ctrl Pts',(-1.88556644576554,-2.92296245069324,
-6.66332850899462));
#17424=CARTESIAN_POINT('Ctrl Pts',(1.43705815184215,-3.16803445271144,-6.50440663399462));
#17425=CARTESIAN_POINT('Ctrl Pts',(3.441053991285,-0.507496356175199,-6.3454847589946));
#17426=CARTESIAN_POINT('Ctrl Pts',(2.29033015795609,2.61799608134706,-6.18656288399462));
#17427=CARTESIAN_POINT('Ctrl Pts',(-0.960728247494492,3.34316533453242,
-6.02764100899461));
#17428=CARTESIAN_POINT('Ctrl Pts',(-3.33072964105243,1.00277406201306,-5.86871913399463));
#17429=CARTESIAN_POINT('Ctrl Pts',(-2.64674860785167,-2.25703793944323,
-5.7097972589946));
#17430=CARTESIAN_POINT('Ctrl Pts',(0.464157708520523,-3.44732825394955,
-5.55087538399462));
#17431=CARTESIAN_POINT('Ctrl Pts',(3.14944377880805,-1.4766378820061,-5.39195350899461));
#17432=CARTESIAN_POINT('Ctrl Pts',(2.94691398666802,1.84802123108039,-5.23303163399462));
#17433=CARTESIAN_POINT('Ctrl Pts',(0.0422591351929435,3.47817457462115,
-5.07410975899461));
#17434=CARTESIAN_POINT('Ctrl Pts',(-2.90114173717657,1.91907610513589,-4.91518788399462));
#17435=CARTESIAN_POINT('Ctrl Pts',(-3.18439425308528,-1.39968359822352,
-4.75626600899461));
#17436=CARTESIAN_POINT('Ctrl Pts',(-0.547772933745816,-3.43502916066676,
-4.59734413399462));
#17437=CARTESIAN_POINT('Ctrl Pts',(2.59111854438333,-2.32068615441235,-4.43842225899462));
#17438=CARTESIAN_POINT('Ctrl Pts',(3.35413063730339,0.921568160892088,-4.27950038399461));
#17439=CARTESIAN_POINT('Ctrl Pts',(1.04163280715265,3.31880719429335,-4.12057850899462));
#17440=CARTESIAN_POINT('Ctrl Pts',(-2.22597145252513,2.67292556353571,-3.96165663399461));
#17441=CARTESIAN_POINT('Ctrl Pts',(-3.45251121700612,-0.423847108822882,
-3.80273475899462));
#17442=CARTESIAN_POINT('Ctrl Pts',(-1.51333284464627,-3.13198080421993,
-3.64381288399462));
#17443=CARTESIAN_POINT('Ctrl Pts',(1.81346887772297,-2.96830097163666,-3.48489100899461));
#17444=CARTESIAN_POINT('Ctrl Pts',(3.47744290446113,-0.0828909096360698,
-3.32596913399462));
#17445=CARTESIAN_POINT('Ctrl Pts',(1.95283814292696,2.87852449403166,-3.16704725899461));
#17446=CARTESIAN_POINT('Ctrl Pts',(-1.36238645797847,3.20052856803004,-3.00812538399462));
#17447=CARTESIAN_POINT('Ctrl Pts',(-3.42839528483007,0.587865519302596,
-2.84920350899461));
#17448=CARTESIAN_POINT('Ctrl Pts',(-2.35079864734157,-2.5638303233491,-2.69028163399462));
#17449=CARTESIAN_POINT('Ctrl Pts',(0.882320542149611,-3.36466788839986,
-2.53135975899461));
#17450=CARTESIAN_POINT('Ctrl Pts',(3.30641181392608,-1.0803339475854,-2.37243788399462));
#17451=CARTESIAN_POINT('Ctrl Pts',(2.69874809340406,2.19459327953189,-2.21351600899462));
#17452=CARTESIAN_POINT('Ctrl Pts',(-0.383484018455407,3.45722670417789,
-2.05459413399462));
#17453=CARTESIAN_POINT('Ctrl Pts',(-3.11408769205621,1.54982000639825,-1.89567225899462));
#17454=CARTESIAN_POINT('Ctrl Pts',(-2.98928396045057,-1.77866970490208,
-1.73675038399462));
#17455=CARTESIAN_POINT('Ctrl Pts',(-0.123511267988871,-3.47623366837271,
-1.57782850899461));
#17456=CARTESIAN_POINT('Ctrl Pts',(2.8555152579241,-1.98634012208901,-1.41890663399462));
#17457=CARTESIAN_POINT('Ctrl Pts',(3.21622379363166,1.32491620962554,-1.25998475899462));
#17458=CARTESIAN_POINT('Ctrl Pts',(0.627882493453467,3.42126867340845,-1.10106288399462));
#17459=CARTESIAN_POINT('Ctrl Pts',(-2.53620118086942,2.38063789554599,-0.942141008994616));
#17460=CARTESIAN_POINT('Ctrl Pts',(-3.3747285883523,-0.843043693618233,
-0.783219133994615));
#17461=CARTESIAN_POINT('Ctrl Pts',(-1.11892083479118,-3.29339054591764,
-0.624297258994616));
#17462=CARTESIAN_POINT('Ctrl Pts',(2.1629791436479,-2.72453659353051,-0.465375383994615));
#17463=CARTESIAN_POINT('Ctrl Pts',(3.46134864158557,0.343709020762119,-0.306453508994615));
#17464=CARTESIAN_POINT('Ctrl Pts',(1.58632847450714,3.0945393904754,-0.147531633994614));
#17465=CARTESIAN_POINT('Ctrl Pts',(-1.74407251151708,3.0122516272526,0.0113902410053857));
#17466=CARTESIAN_POINT('Ctrl Pts',(-3.47370655185682,0.159195307429815,
0.170312116005385));
#17467=CARTESIAN_POINT('Ctrl Pts',(-2.5053913606041,-1.82681981504955,0.276260032672052));
#17468=CARTESIAN_POINT('Ctrl Pts',(-1.70810875200399,-2.39535560853235,
0.329233991005385));
#17469=CARTESIAN_POINT('Ctrl Pts',(2.34668236863854,0.343918483395443,-7.62825));
#17470=CARTESIAN_POINT('Ctrl Pts',(2.23221075339669,1.12500043789087,-7.57527604166667));
#17471=CARTESIAN_POINT('Ctrl Pts',(1.16389372259185,2.55030135594479,-7.469328125));
#17472=CARTESIAN_POINT('Ctrl Pts',(-1.5190222941925,2.35934508271871,-7.31040625));
#17473=CARTESIAN_POINT('Ctrl Pts',(-2.37547941669845,0.786539379620308,
-7.20443357769833));
#17474=CARTESIAN_POINT('Ctrl Pts',(-2.37545665643198,0.00021427761423283,
-7.15143486372999));
#17475=CARTESIAN_POINT('Ctrl Pts',(-2.37545655236239,-0.000153013793341093,
-7.15141010809498));
#17476=CARTESIAN_POINT('Ctrl Pts',(-1.29202279186848,2.64852742499071,1.38777878078145E-15));
#17477=CARTESIAN_POINT('Ctrl Pts',(-1.35199458296097,2.61237463056833,1.3768917757166E-15));
#17478=CARTESIAN_POINT('Ctrl Pts',(-1.41049170787627,2.57398608239727,1.45861512784923E-15));
#17479=CARTESIAN_POINT('Ctrl Pts',(-1.4673716833267,2.53335400329109,3.88578058618805E-16));
#17480=CARTESIAN_POINT('Ctrl Pts',(-1.54687248640264,2.47656278821044,-1.16360444155571E-15));
#17481=CARTESIAN_POINT('Ctrl Pts',(-1.62321595271307,2.41538961241442,-1.82659121223932E-15));
#17482=CARTESIAN_POINT('Ctrl Pts',(-1.69622598732601,2.35021369122793,-1.94289029309402E-15));
#17483=CARTESIAN_POINT('Ctrl Pts',(-1.73503288464287,2.31557084665972,-2.00470654222609E-15));
#17484=CARTESIAN_POINT('Ctrl Pts',(-1.77289731557515,2.27979657283835,-3.6596624852132E-15));
#17485=CARTESIAN_POINT('Ctrl Pts',(-1.80978776603342,2.24294480419717,-4.27435864480685E-15));
#17486=CARTESIAN_POINT('Ctrl Pts',(-1.82764687861092,2.22510441795447,-4.5719404790963E-15));
#17487=CARTESIAN_POINT('Ctrl Pts',(-1.84527766969911,2.207011480151,-6.28754868127402E-15));
#17488=CARTESIAN_POINT('Ctrl Pts',(-1.86267624534788,2.18867199094149,-6.60582699651968E-15));
#17489=CARTESIAN_POINT('Ctrl Pts',(-1.87902498126204,2.17143911671434,-6.9049002211444E-15));
#17490=CARTESIAN_POINT('Ctrl Pts',(-1.8951717260503,2.15398497639697,-1.91704975695889E-15));
#17491=CARTESIAN_POINT('Ctrl Pts',(-1.91109358900524,2.13633667768233,-2.1094237467878E-15));
#17492=CARTESIAN_POINT('Ctrl Pts',(-1.9762348782431,2.06413200324311,-2.89648552145286E-15));
#17493=CARTESIAN_POINT('Ctrl Pts',(-2.03767664102131,1.98861789173561,-5.92176889494793E-15));
#17494=CARTESIAN_POINT('Ctrl Pts',(-2.09524485736161,1.91016955933988,-4.9960036108132E-15));
#17495=CARTESIAN_POINT('Ctrl Pts',(-2.14241512558355,1.84589053323986,-4.23744968054974E-15));
#17496=CARTESIAN_POINT('Ctrl Pts',(-2.1869840436588,1.77964066924168,-3.01258662690371E-15));
#17497=CARTESIAN_POINT('Ctrl Pts',(-2.22883162278026,1.71161678957997,-3.05311331771918E-15));
#17498=CARTESIAN_POINT('Ctrl Pts',(-2.24785166956067,1.68069941274449,-3.07153301059863E-15));
#17499=CARTESIAN_POINT('Ctrl Pts',(-2.26630923741872,1.64941548477482,-1.8357015969624E-15));
#17500=CARTESIAN_POINT('Ctrl Pts',(-2.28419144786431,1.61778322747023,-1.97064586870965E-15));
#17501=CARTESIAN_POINT('Ctrl Pts',(-2.2947105199583,1.5991757965771,-2.05002579366356E-15));
#17502=CARTESIAN_POINT('Ctrl Pts',(-2.30503048226771,1.58044783181963,-2.22291906330319E-15));
#17503=CARTESIAN_POINT('Ctrl Pts',(-2.315148542904,1.56160303675851,-2.13717932240343E-15));
#17504=CARTESIAN_POINT('Ctrl Pts',(-2.32240461406201,1.54808867083041,-2.07569188094589E-15));
#17505=CARTESIAN_POINT('Ctrl Pts',(-2.32955662819893,1.53451447386006,-2.90245848901719E-15));
#17506=CARTESIAN_POINT('Ctrl Pts',(-2.3365973589752,1.52089422682565,-2.88657986402541E-15));
#17507=CARTESIAN_POINT('Ctrl Pts',(-2.38026140223708,1.43642642445602,-2.78810642559811E-15));
#17508=CARTESIAN_POINT('Ctrl Pts',(-2.41971487734872,1.35006846525182,-1.99369284366072E-15));
#17509=CARTESIAN_POINT('Ctrl Pts',(-2.45479279162088,1.26216638421689,-1.97064586870965E-15));
#17510=CARTESIAN_POINT('Ctrl Pts',(-2.49091088104935,1.17165771830431,-1.94691547539493E-15));
#17511=CARTESIAN_POINT('Ctrl Pts',(-2.52239067717506,1.07951100453385,-3.03582794683908E-15));
#17512=CARTESIAN_POINT('Ctrl Pts',(-2.54899471108211,0.986093738756397,
-3.46944695195361E-15));
#17513=CARTESIAN_POINT('Ctrl Pts',(-2.5737480130153,0.899175123570395,-3.87290088661142E-15));
#17514=CARTESIAN_POINT('Ctrl Pts',(-2.59427998939988,0.811155810374791,
-6.26468692693552E-16));
#17515=CARTESIAN_POINT('Ctrl Pts',(-2.61035012881561,0.722335842771595,
-3.05311331771918E-16));
#17516=CARTESIAN_POINT('Ctrl Pts',(-2.6194911252636,0.671813380746323,-1.22631006512308E-16));
#17517=CARTESIAN_POINT('Ctrl Pts',(-2.62718758589052,0.621031999246336,
-2.43292193953287E-15));
#17518=CARTESIAN_POINT('Ctrl Pts',(-2.63338792296817,0.570048893516924,
-2.4980018054066E-15));
#17519=CARTESIAN_POINT('Ctrl Pts',(-2.63582396293746,0.550018227157934,
-2.5235709240657E-15));
#17520=CARTESIAN_POINT('Ctrl Pts',(-2.63802946464811,0.52995046931884,-1.18365939012317E-16));
#17521=CARTESIAN_POINT('Ctrl Pts',(-2.63999815788099,0.509882529321155,
-2.4980018054066E-16));
#17522=CARTESIAN_POINT('Ctrl Pts',(-2.64870462915334,0.421132824610296,
-8.31063136573107E-16));
#17523=CARTESIAN_POINT('Ctrl Pts',(-2.65279857511044,0.332278776698517,
-1.41266709339503E-15));
#17524=CARTESIAN_POINT('Ctrl Pts',(-2.65209667942641,0.24361098136173,-1.2490009027033E-15));
#17525=CARTESIAN_POINT('Ctrl Pts',(-2.65178160418319,0.20380873179956,-1.17553248565223E-15));
#17526=CARTESIAN_POINT('Ctrl Pts',(-2.65049946631159,0.164044057031022,
-2.27209153104153E-15));
#17527=CARTESIAN_POINT('Ctrl Pts',(-2.64823027091117,0.124343747519916,
-2.05391259555654E-15));
#17528=CARTESIAN_POINT('Ctrl Pts',(-2.64306952052804,0.0340547457521929,
-1.55872864938796E-15));
#17529=CARTESIAN_POINT('Ctrl Pts',(-2.63280652105649,-0.0559028803342746,
-7.21832289429463E-16));
#17530=CARTESIAN_POINT('Ctrl Pts',(-2.61763767596916,-0.145196339325471,
-5.55111512312578E-17));
#17531=CARTESIAN_POINT('Ctrl Pts',(-2.60203111097934,-0.237066495747391,
6.30037688348759E-16));
#17532=CARTESIAN_POINT('Ctrl Pts',(-2.58123101177304,-0.32823466497094,
1.60028609533083E-17));
#17533=CARTESIAN_POINT('Ctrl Pts',(-2.55540429049513,-0.418306656786799,
-2.77555756156289E-17));
#17534=CARTESIAN_POINT('Ctrl Pts',(-2.55124208238436,-0.432822567298845,
-3.48076407090747E-17));
#17535=CARTESIAN_POINT('Ctrl Pts',(-2.5469492344459,-0.447309922326401,
2.38273081097328E-16));
#17536=CARTESIAN_POINT('Ctrl Pts',(-2.5425263488523,-0.461766968021027,
2.35922392732846E-16));
#17537=CARTESIAN_POINT('Ctrl Pts',(-2.53834316813649,-0.475440492573617,
2.33699103428367E-16));
#17538=CARTESIAN_POINT('Ctrl Pts',(-2.53404591398863,-0.489079439047373,
-2.93330448010983E-15));
#17539=CARTESIAN_POINT('Ctrl Pts',(-2.5296372776324,-0.502677071255232,
-2.85882428840978E-15));
#17540=CARTESIAN_POINT('Ctrl Pts',(-2.50226678515391,-0.587096347420926,
-2.39642291029584E-15));
#17541=CARTESIAN_POINT('Ctrl Pts',(-2.47058652949289,-0.66999248339392,
8.43465801160117E-16));
#17542=CARTESIAN_POINT('Ctrl Pts',(-2.43480876844775,-0.751061931359657,
4.57966997657877E-16));
#17543=CARTESIAN_POINT('Ctrl Pts',(-2.39908751409446,-0.832003339834344,
7.30770433810818E-17));
#17544=CARTESIAN_POINT('Ctrl Pts',(-2.35928102567076,-0.911124606962677,
-4.15813315017429E-16));
#17545=CARTESIAN_POINT('Ctrl Pts',(-2.31555847154045,-0.988093622425155,
-6.24500451351651E-16));
#17546=CARTESIAN_POINT('Ctrl Pts',(-2.27253682415144,-1.06382876436671,
-8.29842169661056E-16));
#17547=CARTESIAN_POINT('Ctrl Pts',(-2.22572298419624,-1.13748072263154,
8.17918205727042E-18));
#17548=CARTESIAN_POINT('Ctrl Pts',(-2.17524736269965,-1.20869383031328,
-2.77555756156289E-16));
#17549=CARTESIAN_POINT('Ctrl Pts',(-2.15801966745604,-1.2329993798066,-3.75079160327306E-16));
#17550=CARTESIAN_POINT('Ctrl Pts',(-2.14036518691089,-1.25702044358516,
-4.12077394156608E-16));
#17551=CARTESIAN_POINT('Ctrl Pts',(-2.12228847798412,-1.28074161564621,
-3.33066907387547E-16));
#17552=CARTESIAN_POINT('Ctrl Pts',(-2.1108121718594,-1.29580140519709,-2.82905755991096E-16));
#17553=CARTESIAN_POINT('Ctrl Pts',(-2.09916567817787,-1.31074030793348,
-5.65747126062716E-16));
#17554=CARTESIAN_POINT('Ctrl Pts',(-2.08735010827511,-1.3255542322009,-6.31439345255558E-16));
#17555=CARTESIAN_POINT('Ctrl Pts',(-2.07893549744778,-1.33610415984397,
-6.78222908252514E-16));
#17556=CARTESIAN_POINT('Ctrl Pts',(-2.0704406728309,-1.34658373111037,1.09442983389869E-15));
#17557=CARTESIAN_POINT('Ctrl Pts',(-2.06186814397016,-1.35698959226187,
1.03389519168218E-15));
#17558=CARTESIAN_POINT('Ctrl Pts',(-2.0076512765473,-1.42280135021988,6.51044492097758E-16));
#17559=CARTESIAN_POINT('Ctrl Pts',(-1.95030545375966,-1.48569742630702,
-3.12596990479738E-15));
#17560=CARTESIAN_POINT('Ctrl Pts',(-1.88998858415622,-1.54538141434951,
-2.46330733588707E-15));
#17561=CARTESIAN_POINT('Ctrl Pts',(-1.8306216693761,-1.60412541507686,-1.81108130832433E-15));
#17562=CARTESIAN_POINT('Ctrl Pts',(-1.76837591722446,-1.65975822361316,
8.06391941282204E-16));
#17563=CARTESIAN_POINT('Ctrl Pts',(-1.70337601327298,-1.71195478590349,
7.07767178198537E-16));
#17564=CARTESIAN_POINT('Ctrl Pts',(-1.64040340588573,-1.76252337792058,
6.12218444942487E-16));
#17565=CARTESIAN_POINT('Ctrl Pts',(-1.57484520000723,-1.8098670152844,2.93571211404161E-16));
#17566=CARTESIAN_POINT('Ctrl Pts',(-1.50679910444526,-1.85364436762269,
4.66640615037761E-16));
#17567=CARTESIAN_POINT('Ctrl Pts',(-1.46449561434321,-1.88086025379576,
5.7423591118395E-16));
#17568=CARTESIAN_POINT('Ctrl Pts',(-1.42123028569669,-1.90669686113838,
1.15169204501483E-15));
#17569=CARTESIAN_POINT('Ctrl Pts',(-1.37702479013101,-1.93106208855766,
1.11022302462516E-15));
#17570=CARTESIAN_POINT('Origin',(0.,0.,-9.84858989190502));
#17571=CARTESIAN_POINT('Origin',(0.,0.,24.));
#17572=CARTESIAN_POINT('',(-6.,-7.34788079488412E-16,24.));
#17573=CARTESIAN_POINT('Origin',(0.,0.,24.));
#17574=CARTESIAN_POINT('',(-4.,-4.89858719658941E-16,24.));
#17575=CARTESIAN_POINT('Origin',(0.,0.,24.));
#17576=CARTESIAN_POINT('Origin',(0.,0.,24.));
#17577=CARTESIAN_POINT('',(-6.,-7.34788079488412E-16,28.));
#17578=CARTESIAN_POINT('Origin',(0.,0.,28.));
#17579=CARTESIAN_POINT('',(-6.,-7.34788079488412E-16,24.));
#17580=CARTESIAN_POINT('Origin',(0.,0.,28.));
#17581=CARTESIAN_POINT('Origin',(0.,0.,0.));
#17582=CARTESIAN_POINT('',(-4.,-4.89858719658941E-16,0.));
#17583=CARTESIAN_POINT('Origin',(0.,0.,0.));
#17584=CARTESIAN_POINT('Origin',(0.,0.,0.));
#17585=CARTESIAN_POINT('',(-4.,-4.89858719658941E-16,0.));
#17586=CARTESIAN_POINT('Origin',(0.,0.,-8.));
#17587=CARTESIAN_POINT('',(0.,0.,0.));
#17588=CARTESIAN_POINT('Origin',(0.,0.,0.));
#17589=CARTESIAN_POINT('',(-1.95633575083409,0.00127285042835199,0.22586969212423));
#17590=CARTESIAN_POINT('',(-1.95588099269616,0.00206992261158074,0.124130307875763));
#17591=CARTESIAN_POINT('',(-1.954,-2.39295984553393E-16,0.));
#17592=CARTESIAN_POINT('',(0.861525859670522,1.75382131162755,0.));
#17593=CARTESIAN_POINT('Ctrl Pts',(-1.95633575083409,0.00127285042835199,
0.22586969212423));
#17594=CARTESIAN_POINT('Ctrl Pts',(-1.95680045835965,0.0682528464970811,
0.222037453599974));
#17595=CARTESIAN_POINT('Ctrl Pts',(-1.95365942703396,0.135185904981779,
0.218205215075717));
#17596=CARTESIAN_POINT('Ctrl Pts',(-1.94676900820417,0.201727159714737,
0.214372976551461));
#17597=CARTESIAN_POINT('Ctrl Pts',(-1.88017550235509,0.84482528563818,0.1773357216495));
#17598=CARTESIAN_POINT('Ctrl Pts',(-1.46336852822225,1.45132678060953,0.14029846674754));
#17599=CARTESIAN_POINT('Ctrl Pts',(-0.886890238653646,1.74452948919289,
0.103261211845579));
#17600=CARTESIAN_POINT('Ctrl Pts',(-0.351142769057663,2.01701608937305,
0.0688408078970528));
#17601=CARTESIAN_POINT('Ctrl Pts',(0.322510092743222,2.01891187055583,0.0344204039485265));
#17602=CARTESIAN_POINT('Ctrl Pts',(0.86356802035368,1.756414520678,3.12250225675825E-16));
#17603=CARTESIAN_POINT('',(-0.861525859670558,1.75382131162753,0.));
#17604=CARTESIAN_POINT('Origin',(0.,0.,0.));
#17605=CARTESIAN_POINT('Ctrl Pts',(-0.861525859670558,1.75382131162753,
1.42247325030098E-15));
#17606=CARTESIAN_POINT('Ctrl Pts',(-1.44504958508736,1.46717821073411,0.0370673336485529));
#17607=CARTESIAN_POINT('Ctrl Pts',(-1.86921464413225,0.868908493151144,
0.0741346672971042));
#17608=CARTESIAN_POINT('Ctrl Pts',(-1.94383305148301,0.227162278519285,
0.111202000945656));
#17609=CARTESIAN_POINT('Ctrl Pts',(-1.95250816222439,0.152553081171747,
0.115511436589025));
#17610=CARTESIAN_POINT('Ctrl Pts',(-1.95645869249163,0.0773562420658186,
0.119820872232394));
#17611=CARTESIAN_POINT('Ctrl Pts',(-1.95588099269616,0.00206992261158074,
0.124130307875763));
#17612=CARTESIAN_POINT('Origin',(0.,0.,0.));
#17613=CARTESIAN_POINT('',(-1.95128228942929,0.000979822369055472,0.92586969212423));
#17614=CARTESIAN_POINT('',(-1.95119461725619,0.00092642636832007,0.824130307875761));
#17615=CARTESIAN_POINT('',(-1.954,-2.39295984553393E-16,0.));
#17616=CARTESIAN_POINT('Ctrl Pts',(-1.95128228942929,0.000979822369055472,
0.92586969212423));
#17617=CARTESIAN_POINT('Ctrl Pts',(-1.9524734062589,0.263895099571634,0.910927649678405));
#17618=CARTESIAN_POINT('Ctrl Pts',(-1.90305436999396,0.526380727998823,
0.89598560723258));
#17619=CARTESIAN_POINT('Ctrl Pts',(-1.80089851330331,0.766421656018886,
0.881043564786755));
#17620=CARTESIAN_POINT('Ctrl Pts',(-1.54768195889331,1.36141775981235,0.844006309884795));
#17621=CARTESIAN_POINT('Ctrl Pts',(-0.97044557322541,1.81851157863974,0.806969054982833));
#17622=CARTESIAN_POINT('Ctrl Pts',(-0.333248418269387,1.92861710553695,
0.769931800080872));
#17623=CARTESIAN_POINT('Ctrl Pts',(0.303948736686636,2.03872263243416,0.732894545178912));
#17624=CARTESIAN_POINT('Ctrl Pts',(1.00110666093079,1.80183986740118,0.695857290276951));
#17625=CARTESIAN_POINT('Ctrl Pts',(1.43929923459321,1.3263033286824,0.658820035374991));
#17626=CARTESIAN_POINT('Ctrl Pts',(1.87749180825564,0.850766789963622,0.62178278047303));
#17627=CARTESIAN_POINT('Ctrl Pts',(2.05671903133634,0.136576477559035,0.584745525571069));
#17628=CARTESIAN_POINT('Ctrl Pts',(1.89500173497496,-0.48949878222732,0.547708270669108));
#17629=CARTESIAN_POINT('Ctrl Pts',(1.73328443861357,-1.11557404201368,0.510671015767147));
#17630=CARTESIAN_POINT('Ctrl Pts',(1.23062262281009,-1.65353424918181,0.473633760865186));
#17631=CARTESIAN_POINT('Ctrl Pts',(0.616944482209929,-1.85739202336751,
0.436596505963226));
#17632=CARTESIAN_POINT('Ctrl Pts',(0.00326634160977092,-2.06124979755321,
0.399559251061265));
#17633=CARTESIAN_POINT('Ctrl Pts',(-0.721428123787067,-1.93100513875649,
0.362521996159304));
#17634=CARTESIAN_POINT('Ctrl Pts',(-1.22558533770282,-1.52603543092037,
0.325484741257344));
#17635=CARTESIAN_POINT('Ctrl Pts',(-1.67757748964075,-1.16296787052023,
0.292279724879639));
#17636=CARTESIAN_POINT('Ctrl Pts',(-1.95230922145719,-0.579085562119143,
0.259074708501934));
#17637=CARTESIAN_POINT('Ctrl Pts',(-1.95633575083409,0.00127285042835199,
0.22586969212423));
#17638=CARTESIAN_POINT('Ctrl Pts',(-1.95588099269616,0.00206992261158074,
0.124130307875763));
#17639=CARTESIAN_POINT('Ctrl Pts',(-1.95148964483908,-0.570214194837128,
0.156888205880946));
#17640=CARTESIAN_POINT('Ctrl Pts',(-1.68544890035158,-1.14766865010464,
0.189646103886129));
#17641=CARTESIAN_POINT('Ctrl Pts',(-1.24400073481116,-1.51148858380038,
0.222404001891312));
#17642=CARTESIAN_POINT('Ctrl Pts',(-0.744478255131947,-1.9231705198074,
0.259471335539864));
#17643=CARTESIAN_POINT('Ctrl Pts',(-0.0203615401169106,-2.06131168014067,
0.296538669188416));
#17644=CARTESIAN_POINT('Ctrl Pts',(0.596117854997422,-1.86404025704795,
0.333606002836968));
#17645=CARTESIAN_POINT('Ctrl Pts',(1.21259725011176,-1.66676883395523,0.37067333648552));
#17646=CARTESIAN_POINT('Ctrl Pts',(1.72143932532539,-1.13408482743652,0.407740670134072));
#17647=CARTESIAN_POINT('Ctrl Pts',(1.88977433415544,-0.509313521695289,
0.444808003782624));
#17648=CARTESIAN_POINT('Ctrl Pts',(2.05810934298549,0.115457784045944,0.481875337431176));
#17649=CARTESIAN_POINT('Ctrl Pts',(1.88593728543196,0.832316389009701,0.518942671079728));
#17650=CARTESIAN_POINT('Ctrl Pts',(1.45200572115437,1.31246709551687,0.55601000472828));
#17651=CARTESIAN_POINT('Ctrl Pts',(1.01807415687679,1.79261780202404,0.593077338376832));
#17652=CARTESIAN_POINT('Ctrl Pts',(0.322383085875136,2.03606061007462,0.630144672025384));
#17653=CARTESIAN_POINT('Ctrl Pts',(-0.316275274467243,1.93146093707914,
0.667212005673936));
#17654=CARTESIAN_POINT('Ctrl Pts',(-0.954933634809622,1.82686126408366,
0.704279339322488));
#17655=CARTESIAN_POINT('Ctrl Pts',(-1.53655928449273,1.37421911004211,0.741346672971039));
#17656=CARTESIAN_POINT('Ctrl Pts',(-1.79472283882274,0.780804664464737,
0.778414006619591));
#17657=CARTESIAN_POINT('Ctrl Pts',(-1.9008565659387,0.53684580281587,0.793652773704981));
#17658=CARTESIAN_POINT('Ctrl Pts',(-1.95232138952433,0.269094766021062,
0.808891540790371));
#17659=CARTESIAN_POINT('Ctrl Pts',(-1.95119461725619,0.00092642636832007,
0.824130307875761));
#17660=CARTESIAN_POINT('Origin',(0.,0.,0.));
#17661=CARTESIAN_POINT('',(-1.95279539392324,-0.00168116113097749,1.62586969212423));
#17662=CARTESIAN_POINT('',(-1.95283689833027,-0.00169757742976787,1.52413030787576));
#17663=CARTESIAN_POINT('',(-1.954,-2.39295984553393E-16,0.));
#17664=CARTESIAN_POINT('Ctrl Pts',(-1.95279539392324,-0.00168116113097749,
1.62586969212423));
#17665=CARTESIAN_POINT('Ctrl Pts',(-1.94903666796486,0.455824327828861,
1.59981784575684));
#17666=CARTESIAN_POINT('Ctrl Pts',(-1.78857561082415,0.915704606010159,
1.57376599938944));
#17667=CARTESIAN_POINT('Ctrl Pts',(-1.49502845554474,1.26314111490869,1.54771415302205));
#17668=CARTESIAN_POINT('Ctrl Pts',(-1.07769984618227,1.75708286325356,1.51067689812009));
#17669=CARTESIAN_POINT('Ctrl Pts',(-0.391383019514876,2.02375783115006,
1.47363964321813));
#17670=CARTESIAN_POINT('Ctrl Pts',(0.249960502791804,1.9411735695446,1.43660238831617));
#17671=CARTESIAN_POINT('Ctrl Pts',(0.891304025098484,1.85858930793915,1.39956513341421));
#17672=CARTESIAN_POINT('Ctrl Pts',(1.48767424304445,1.42674581683174,1.36252787851224));
#17673=CARTESIAN_POINT('Ctrl Pts',(1.76625632450792,0.843193022913364,1.32549062361028));
#17674=CARTESIAN_POINT('Ctrl Pts',(2.04483840597138,0.259640228994984,1.28845336870832));
#17675=CARTESIAN_POINT('Ctrl Pts',(2.00563235095235,-0.475621867734372,
1.25141611380636));
#17676=CARTESIAN_POINT('Ctrl Pts',(1.66657351619212,-1.026240070129,1.2143788589044));
#17677=CARTESIAN_POINT('Ctrl Pts',(1.32751468143189,-1.57685827252363,1.17734160400244));
#17678=CARTESIAN_POINT('Ctrl Pts',(0.688603066930477,-1.94283258058353,
1.14030434910048));
#17679=CARTESIAN_POINT('Ctrl Pts',(0.0421139319386674,-1.95674712405518,
1.10326709419852));
#17680=CARTESIAN_POINT('Ctrl Pts',(-0.604375203053146,-1.97066166752684,
1.06622983929656));
#17681=CARTESIAN_POINT('Ctrl Pts',(-1.25844185853535,-1.63251644641023,
1.0291925843946));
#17682=CARTESIAN_POINT('Ctrl Pts',(-1.62087682470039,-1.09699464147216,
0.992155329492637));
#17683=CARTESIAN_POINT('Ctrl Pts',(-1.83709364746835,-0.777519883250448,
0.970060117036501));
#17684=CARTESIAN_POINT('Ctrl Pts',(-1.94952095194778,-0.387800287767629,
0.947964904580365));
#17685=CARTESIAN_POINT('Ctrl Pts',(-1.95128228942929,0.000979822369055472,
0.92586969212423));
#17686=CARTESIAN_POINT('Ctrl Pts',(-1.95119461725619,0.00092642636832007,
0.824130307875761));
#17687=CARTESIAN_POINT('Ctrl Pts',(-1.94958058750438,-0.38320769809472,
0.845958874438923));
#17688=CARTESIAN_POINT('Ctrl Pts',(-1.84005520872064,-0.768198075607766,
0.867787441002085));
#17689=CARTESIAN_POINT('Ctrl Pts',(-1.62872406172904,-1.08534175300753,
0.889616007565247));
#17690=CARTESIAN_POINT('Ctrl Pts',(-1.26986027132842,-1.62388698778921,
0.926683341213799));
#17691=CARTESIAN_POINT('Ctrl Pts',(-0.617431231550254,-1.96679072023937,
0.963750674862351));
#17692=CARTESIAN_POINT('Ctrl Pts',(0.0296497544693555,-1.9569836764894,
1.0008180085109));
#17693=CARTESIAN_POINT('Ctrl Pts',(0.676730740488965,-1.94717663273943,
1.03788534215945));
#17694=CARTESIAN_POINT('Ctrl Pts',(1.31846367275002,-1.58465881278932,1.07495267580801));
#17695=CARTESIAN_POINT('Ctrl Pts',(1.66085075139256,-1.03549895096933,1.11202000945656));
#17696=CARTESIAN_POINT('Ctrl Pts',(2.00323783003509,-0.486339089149333,
1.14908734310511));
#17697=CARTESIAN_POINT('Ctrl Pts',(2.04627905505911,0.249462814540552,1.18615467675366));
#17698=CARTESIAN_POINT('Ctrl Pts',(1.77025280539679,0.834799217616478,1.22322201040222));
#17699=CARTESIAN_POINT('Ctrl Pts',(1.49422655573448,1.4201356206924,1.26028934405077));
#17700=CARTESIAN_POINT('Ctrl Pts',(0.899132831385847,1.85500652315437,1.29735667769932));
#17701=CARTESIAN_POINT('Ctrl Pts',(0.257608856151057,1.94018461251091,1.33442401134787));
#17702=CARTESIAN_POINT('Ctrl Pts',(-0.383915119083735,2.02536270186746,
1.37149134499642));
#17703=CARTESIAN_POINT('Ctrl Pts',(-1.07186934520468,1.76084797811858,1.40855867864497));
#17704=CARTESIAN_POINT('Ctrl Pts',(-1.49107575958572,1.26782285617356,1.44562601229353));
#17705=CARTESIAN_POINT('Ctrl Pts',(-1.78701921370236,0.919766260307501,
1.47179411082094));
#17706=CARTESIAN_POINT('Ctrl Pts',(-1.94902381498454,0.457824381443284,
1.49796220934835));
#17707=CARTESIAN_POINT('Ctrl Pts',(-1.95283689833027,-0.00169757742976787,
1.52413030787576));
#17708=CARTESIAN_POINT('Origin',(0.,0.,0.));
#17709=CARTESIAN_POINT('',(-1.95719985818546,4.05420783899653E-5,2.32586969212423));
#17710=CARTESIAN_POINT('',(-1.95721255371923,9.84009623044488E-6,2.22413030787576));
#17711=CARTESIAN_POINT('',(-1.954,-2.39295984553393E-16,0.));
#17712=CARTESIAN_POINT('Ctrl Pts',(-1.95719985818546,4.05420783900091E-5,
2.32586969212423));
#17713=CARTESIAN_POINT('Ctrl Pts',(-1.95720052181173,0.00221238218774959,
2.32574529673723));
#17714=CARTESIAN_POINT('Ctrl Pts',(-1.95719721915126,0.00438422021875816,
2.32562090135023));
#17715=CARTESIAN_POINT('Ctrl Pts',(-1.95718994413828,0.00655604494350104,
2.32549650596323));
#17716=CARTESIAN_POINT('Ctrl Pts',(-1.95502389508506,0.653191164393938,
2.28845925106126));
#17717=CARTESIAN_POINT('Ctrl Pts',(-1.6007166691436,1.2986467097638,2.2514219961593));
#17718=CARTESIAN_POINT('Ctrl Pts',(-1.05634917726868,1.64765344582725,2.21438474125734));
#17719=CARTESIAN_POINT('Ctrl Pts',(-0.511981685393759,1.9966601818907,2.17734748635538));
#17720=CARTESIAN_POINT('Ctrl Pts',(0.222446072414618,2.04921810864774,2.14031023145342));
#17721=CARTESIAN_POINT('Ctrl Pts',(0.810963756254723,1.78128415395532,2.10327297655146));
#17722=CARTESIAN_POINT('Ctrl Pts',(1.39948144009482,1.51335019926291,2.0662357216495));
#17723=CARTESIAN_POINT('Ctrl Pts',(1.84208904996665,0.924924363121033,2.02919846674754));
#17724=CARTESIAN_POINT('Ctrl Pts',(1.93631189757409,0.285187129558038,1.99216121184558));
#17725=CARTESIAN_POINT('Ctrl Pts',(2.03053474518152,-0.354550104004963,
1.95512395694362));
#17726=CARTESIAN_POINT('Ctrl Pts',(1.77637283052455,-1.04559873498909,1.91808670204166));
#17727=CARTESIAN_POINT('Ctrl Pts',(1.29009472793977,-1.47183255494777,1.8810494471397));
#17728=CARTESIAN_POINT('Ctrl Pts',(0.803816625355003,-1.89806637490645,
1.84401219223774));
#17729=CARTESIAN_POINT('Ctrl Pts',(0.0854223348424371,-2.05948538383969,
1.80697493733577));
#17730=CARTESIAN_POINT('Ctrl Pts',(-0.536452459305869,-1.88224710468127,
1.76993768243381));
#17731=CARTESIAN_POINT('Ctrl Pts',(-1.15832725345417,-1.70500882552285,
1.73290042753185));
#17732=CARTESIAN_POINT('Ctrl Pts',(-1.68368255123822,-1.18911325827277,
1.69586317262989));
#17733=CARTESIAN_POINT('Ctrl Pts',(-1.87219000410148,-0.570561210251106,
1.65882591772793));
#17734=CARTESIAN_POINT('Ctrl Pts',(-1.92810212250753,-0.387096021877988,
1.64784050919336));
#17735=CARTESIAN_POINT('Ctrl Pts',(-1.95438035414602,-0.194599721764027,
1.6368551006588));
#17736=CARTESIAN_POINT('Ctrl Pts',(-1.95279539392324,-0.00168116113097727,
1.62586969212423));
#17737=CARTESIAN_POINT('Ctrl Pts',(-1.95283689833027,-0.00169757742976787,
1.52413030787576));
#17738=CARTESIAN_POINT('Ctrl Pts',(-1.95442507990479,-0.193092373189868,
1.5350295429969));
#17739=CARTESIAN_POINT('Ctrl Pts',(-1.92857030457963,-0.38406736287639,
1.54592877811804));
#17740=CARTESIAN_POINT('Ctrl Pts',(-1.87352018127017,-0.566218843228074,
1.55682801323918));
#17741=CARTESIAN_POINT('Ctrl Pts',(-1.68629958593245,-1.18569990054353,
1.59389534688773));
#17742=CARTESIAN_POINT('Ctrl Pts',(-1.16139979261586,-1.70312649503327,
1.63096268053629));
#17743=CARTESIAN_POINT('Ctrl Pts',(-0.539298197806726,-1.88144579938109,
1.66803001418484));
#17744=CARTESIAN_POINT('Ctrl Pts',(0.0828033970024101,-2.0597651037289,
1.70509734783339));
#17745=CARTESIAN_POINT('Ctrl Pts',(0.802106793304097,-1.89897711793479,
1.74216468148194));
#17746=CARTESIAN_POINT('Ctrl Pts',(1.28907099594446,-1.47274481385923,1.77923201513049));
#17747=CARTESIAN_POINT('Ctrl Pts',(1.77603519858483,-1.04651250978366,1.81629934877905));
#17748=CARTESIAN_POINT('Ctrl Pts',(2.03066020756387,-0.35483588742664,1.8533666824276));
#17749=CARTESIAN_POINT('Ctrl Pts',(1.9362922595033,0.285400693385207,1.89043401607615));
#17750=CARTESIAN_POINT('Ctrl Pts',(1.84192431144273,0.925637274197054,1.9275013497247));
#17751=CARTESIAN_POINT('Ctrl Pts',(1.39856340634255,1.51443381346373,1.96456868337325));
#17752=CARTESIAN_POINT('Ctrl Pts',(0.809330598539892,1.78203960359444,2.00163601702181));
#17753=CARTESIAN_POINT('Ctrl Pts',(0.220097790737234,2.04964539372514,2.03870335067036));
#17754=CARTESIAN_POINT('Ctrl Pts',(-0.515006919767895,1.99606043471988,
2.07577068431891));
#17755=CARTESIAN_POINT('Ctrl Pts',(-1.05920324210055,1.6458340532769,2.11283801796746));
#17756=CARTESIAN_POINT('Ctrl Pts',(-1.60384141728657,1.29532331025408,2.1499354479369));
#17757=CARTESIAN_POINT('Ctrl Pts',(-1.95726085438506,0.64768924107042,2.18703287790633));
#17758=CARTESIAN_POINT('Ctrl Pts',(-1.95721255371923,9.84009623044488E-6,
2.22413030787576));
#17759=CARTESIAN_POINT('Origin',(0.,0.,0.));
#17760=CARTESIAN_POINT('',(-1.95267758926504,0.00165506900100115,3.02586969212423));
#17761=CARTESIAN_POINT('',(-1.95280791655641,0.00169181170498602,2.92413030787576));
#17762=CARTESIAN_POINT('',(-1.954,-2.39295984553393E-16,0.));
#17763=CARTESIAN_POINT('Ctrl Pts',(-1.95267758926504,0.00165506900100115,
3.02586969212423));
#17764=CARTESIAN_POINT('Ctrl Pts',(-1.95426628302477,0.198972830964143,
3.01463549281566));
#17765=CARTESIAN_POINT('Ctrl Pts',(-1.92675962108266,0.395857959120396,
3.00340129350709));
#17766=CARTESIAN_POINT('Ctrl Pts',(-1.86832558386105,0.583090877542938,
2.99216709419852));
#17767=CARTESIAN_POINT('Ctrl Pts',(-1.67567844701734,1.20036613990759,2.95512983929656));
#17768=CARTESIAN_POINT('Ctrl Pts',(-1.14687877096073,1.7127306304502,2.9180925843946));
#17769=CARTESIAN_POINT('Ctrl Pts',(-0.52383054918719,1.88579877362532,2.88105532949264));
#17770=CARTESIAN_POINT('Ctrl Pts',(0.0992176725863465,2.05886691680043,
2.84401807459068));
#17771=CARTESIAN_POINT('Ctrl Pts',(0.81651444007682,1.89263871260806,2.80698081968871));
#17772=CARTESIAN_POINT('Ctrl Pts',(1.29992613215786,1.46315669344762,2.76994356478675));
#17773=CARTESIAN_POINT('Ctrl Pts',(1.7833378242389,1.03367467428718,2.73290630988479));
#17774=CARTESIAN_POINT('Ctrl Pts',(2.03286444091049,0.340938840158676,2.69586905498283));
#17775=CARTESIAN_POINT('Ctrl Pts',(1.93435786935885,-0.298152799828459,
2.65883180008087));
#17776=CARTESIAN_POINT('Ctrl Pts',(1.8358512978072,-0.937244439815588,2.62179454517891));
#17777=CARTESIAN_POINT('Ctrl Pts',(1.38931153803231,-1.52269188566136,2.58475729027695));
#17778=CARTESIAN_POINT('Ctrl Pts',(0.799012072181727,-1.78667713026121,
2.54772003537499));
#17779=CARTESIAN_POINT('Ctrl Pts',(0.208712606331136,-2.05066237486107,
2.51068278047303));
#17780=CARTESIAN_POINT('Ctrl Pts',(-0.525346565595159,-1.99318541821502,
2.47364552557107));
#17781=CARTESIAN_POINT('Ctrl Pts',(-1.06736371547582,-1.64053959312649,
2.43660827066911));
#17782=CARTESIAN_POINT('Ctrl Pts',(-1.60756041637074,-1.28907818394574,
2.39969541115415));
#17783=CARTESIAN_POINT('Ctrl Pts',(-1.95700293493792,-0.644427317850318,
2.36278255163919));
#17784=CARTESIAN_POINT('Ctrl Pts',(-1.95719985818546,4.05420783899653E-5,
2.32586969212423));
#17785=CARTESIAN_POINT('Ctrl Pts',(-1.95721255371923,9.84009623044488E-6,
2.22413030787576));
#17786=CARTESIAN_POINT('Ctrl Pts',(-1.95716433142391,-0.646618665056022,
2.26116754520343));
#17787=CARTESIAN_POINT('Ctrl Pts',(-1.60505607381363,-1.29329214304674,
2.2982047825311));
#17788=CARTESIAN_POINT('Ctrl Pts',(-1.0618695239415,-1.64411505913035,2.33524201985877));
#17789=CARTESIAN_POINT('Ctrl Pts',(-0.518241582705361,-1.99522305260678,
2.37230935350733));
#17790=CARTESIAN_POINT('Ctrl Pts',(0.216775315978968,-2.04999947469641,
2.40937668715588));
#17791=CARTESIAN_POINT('Ctrl Pts',(0.806441097699488,-1.78334909096271,
2.44644402080443));
#17792=CARTESIAN_POINT('Ctrl Pts',(1.39610687942001,-1.516698707229,2.48351135445298));
#17793=CARTESIAN_POINT('Ctrl Pts',(1.84042154417672,-0.928621517671956,
2.52057868810153));
#17794=CARTESIAN_POINT('Ctrl Pts',(1.93582711194427,-0.288538757100728,
2.55764602175009));
#17795=CARTESIAN_POINT('Ctrl Pts',(2.03123267971181,0.351544003470497,2.59471335539864));
#17796=CARTESIAN_POINT('Ctrl Pts',(1.77772915049019,1.04363233505591,2.63178068904719));
#17797=CARTESIAN_POINT('Ctrl Pts',(1.29145643683783,1.470653423467,2.66884802269574));
#17798=CARTESIAN_POINT('Ctrl Pts',(0.805183723185476,1.89767451187809,2.7059153563443));
#17799=CARTESIAN_POINT('Ctrl Pts',(0.0861418251023859,2.05962835711487,
2.74298268999285));
#17800=CARTESIAN_POINT('Ctrl Pts',(-0.53624795552402,1.882317548121,2.7800500236414));
#17801=CARTESIAN_POINT('Ctrl Pts',(-1.15863773615042,1.70500673912713,2.81711735728995));
#17802=CARTESIAN_POINT('Ctrl Pts',(-1.68437539932014,1.18843127590261,2.8541846909385));
#17803=CARTESIAN_POINT('Ctrl Pts',(-1.87259989616401,0.569254644402596,
2.89125202458705));
#17804=CARTESIAN_POINT('Ctrl Pts',(-1.92825085816542,0.386187212853816,
2.90221145234996));
#17805=CARTESIAN_POINT('Ctrl Pts',(-1.95439762435419,0.194150753541291,
2.91317088011286));
#17806=CARTESIAN_POINT('Ctrl Pts',(-1.95280791655641,0.00169181170498602,
2.92413030787576));
#17807=CARTESIAN_POINT('Origin',(0.,0.,0.));
#17808=CARTESIAN_POINT('',(-1.95135083467133,-0.00103713828173369,3.72586969212423));
#17809=CARTESIAN_POINT('',(-1.95121488712599,-0.000926387452031019,3.62413030787576));
#17810=CARTESIAN_POINT('',(-1.954,-2.39295984553393E-16,0.));
#17811=CARTESIAN_POINT('Ctrl Pts',(-1.95135083467133,-0.00103713828173369,
3.72586969212423));
#17812=CARTESIAN_POINT('Ctrl Pts',(-1.94945690425454,0.392085240919391,
3.70352568889409));
#17813=CARTESIAN_POINT('Ctrl Pts',(-1.83430205983262,0.786228342622907,
3.68118168566395));
#17814=CARTESIAN_POINT('Ctrl Pts',(-1.61349106342003,1.10782762515327,3.65883768243382));
#17815=CARTESIAN_POINT('Ctrl Pts',(-1.24747638489286,1.64090822314112,3.62180042753185));
#17816=CARTESIAN_POINT('Ctrl Pts',(-0.591159457848277,1.9746664586804,3.58476317262989));
#17817=CARTESIAN_POINT('Ctrl Pts',(0.0552218529205667,1.95642173514589,
3.54772591772793));
#17818=CARTESIAN_POINT('Ctrl Pts',(0.70160316368942,1.93817701161139,3.51068866282597));
#17819=CARTESIAN_POINT('Ctrl Pts',(1.33804885818252,1.5679293290031,3.47365140792401));
#17820=CARTESIAN_POINT('Ctrl Pts',(1.67341133910821,1.01505169766431,3.43661415302205));
#17821=CARTESIAN_POINT('Ctrl Pts',(2.0087738200339,0.462174066325523,3.39957689812009));
#17822=CARTESIAN_POINT('Ctrl Pts',(2.04305308739216,-0.273333513743766,
3.36253964321813));
#17823=CARTESIAN_POINT('Ctrl Pts',(1.76056779332365,-0.855006727399908,
3.32550238831617));
#17824=CARTESIAN_POINT('Ctrl Pts',(1.47808249925514,-1.43667994105605,3.2884651334142));
#17825=CARTESIAN_POINT('Ctrl Pts',(0.878832643759864,-1.86451878829905,
3.25142787851224));
#17826=CARTESIAN_POINT('Ctrl Pts',(0.236950265307058,-1.94280468152938,
3.21439062361029));
#17827=CARTESIAN_POINT('Ctrl Pts',(-0.404932113145755,-2.02109057475972,
3.17735336870832));
#17828=CARTESIAN_POINT('Ctrl Pts',(-1.0894470145561,-1.74982351397736,3.14031611380636));
#17829=CARTESIAN_POINT('Ctrl Pts',(-1.50345716644585,-1.25309696649286,
3.1032788589044));
#17830=CARTESIAN_POINT('Ctrl Pts',(-1.7918890978543,-0.907038308706706,
3.07747580331101));
#17831=CARTESIAN_POINT('Ctrl Pts',(-1.94902862841993,-0.451550454744232,
3.05167274771762));
#17832=CARTESIAN_POINT('Ctrl Pts',(-1.95267758926504,0.00165506900100115,
3.02586969212423));
#17833=CARTESIAN_POINT('Ctrl Pts',(-1.95280791655641,0.00169181170498602,
2.92413030787576));
#17834=CARTESIAN_POINT('Ctrl Pts',(-1.94902086284632,-0.456790150037774,
2.95023821376141));
#17835=CARTESIAN_POINT('Ctrl Pts',(-1.78782842975758,-0.917669713651943,
2.97634611964706));
#17836=CARTESIAN_POINT('Ctrl Pts',(-1.49312888403822,-1.26540402906769,
3.00245402553271));
#17837=CARTESIAN_POINT('Ctrl Pts',(-1.07472204455054,-1.75910827126244,
3.03952135918126));
#17838=CARTESIAN_POINT('Ctrl Pts',(-0.387197035057166,-2.02473895587643,
3.07658869282981));
#17839=CARTESIAN_POINT('Ctrl Pts',(0.254463965370863,-1.94060024520244,
3.11365602647837));
#17840=CARTESIAN_POINT('Ctrl Pts',(0.896124965798891,-1.85646153452846,
3.15072336012692));
#17841=CARTESIAN_POINT('Ctrl Pts',(1.49192195716157,-1.42255342856649,3.18779069377547));
#17842=CARTESIAN_POINT('Ctrl Pts',(1.76889696399884,-0.837666253363929,
3.22485802742402));
#17843=CARTESIAN_POINT('Ctrl Pts',(2.04587197083611,-0.252779078161363,
3.26192536107257));
#17844=CARTESIAN_POINT('Ctrl Pts',(2.00402499314796,0.483087166281804,3.29899269472113));
#17845=CARTESIAN_POINT('Ctrl Pts',(1.66252777312397,1.03280328468034,3.33606002836968));
#17846=CARTESIAN_POINT('Ctrl Pts',(1.32103055309999,1.58251940307888,3.37312736201823));
#17847=CARTESIAN_POINT('Ctrl Pts',(0.679883090740172,1.94608539543278,3.41019469566678));
#17848=CARTESIAN_POINT('Ctrl Pts',(0.0328201913788997,1.95693741757976,
3.44726202931533));
#17849=CARTESIAN_POINT('Ctrl Pts',(-0.614242707982372,1.96778943972675,
3.48432936296388));
#17850=CARTESIAN_POINT('Ctrl Pts',(-1.2672210443451,1.62592749166683,3.52139669661244));
#17851=CARTESIAN_POINT('Ctrl Pts',(-1.62695982484692,1.08797194339114,3.55846403026099));
#17852=CARTESIAN_POINT('Ctrl Pts',(-1.83939041447971,0.770301954748211,
3.58035278946591));
#17853=CARTESIAN_POINT('Ctrl Pts',(-1.94956657085447,0.384252923937107,
3.60224154867084));
#17854=CARTESIAN_POINT('Ctrl Pts',(-1.95121488712599,-0.000926387452031019,
3.62413030787576));
#17855=CARTESIAN_POINT('Origin',(0.,0.,0.));
#17856=CARTESIAN_POINT('',(-1.95645531603829,-0.0010761721163155,4.42586969212423));
#17857=CARTESIAN_POINT('',(-1.95619906720822,-0.0012405029508829,4.32413030787576));
#17858=CARTESIAN_POINT('',(-1.954,-2.39295984553393E-16,0.));
#17859=CARTESIAN_POINT('Ctrl Pts',(-1.95645531603829,-0.0010761721163155,
4.42586969212423));
#17860=CARTESIAN_POINT('Ctrl Pts',(-1.95258058399789,0.583590658408003,
4.39241588497252));
#17861=CARTESIAN_POINT('Ctrl Pts',(-1.67315132747224,1.17147065165432,4.35896207782082));
#17862=CARTESIAN_POINT('Ctrl Pts',(-1.21532426049127,1.53415201354063,4.32550827066911));
#17863=CARTESIAN_POINT('Ctrl Pts',(-0.708456456061838,1.93568245781738,
4.28847101576715));
#17864=CARTESIAN_POINT('Ctrl Pts',(0.0170747010795776,2.06118547981998,
4.25143376086519));
#17865=CARTESIAN_POINT('Ctrl Pts',(0.629368696890541,1.85324863473949,4.21439650596323));
#17866=CARTESIAN_POINT('Ctrl Pts',(1.2416626927015,1.64531178965899,4.17735925106126));
#17867=CARTESIAN_POINT('Ctrl Pts',(1.740719527182,1.10393507749541,4.1403219961593));
#17868=CARTESIAN_POINT('Ctrl Pts',(1.89824132742874,0.476775965869676,4.10328474125734));
#17869=CARTESIAN_POINT('Ctrl Pts',(2.05576312767549,-0.15038314575607,4.06624748635538));
#17870=CARTESIAN_POINT('Ctrl Pts',(1.87174989368847,-0.863324656843973,
4.02921023145342));
#17871=CARTESIAN_POINT('Ctrl Pts',(1.43038007369796,-1.33590729601914,3.99217297655146));
#17872=CARTESIAN_POINT('Ctrl Pts',(0.989010253707457,-1.80848993519431,
3.9551357216495));
#17873=CARTESIAN_POINT('Ctrl Pts',(0.290283847713488,-2.04071370245675,
3.91809846674754));
#17874=CARTESIAN_POINT('Ctrl Pts',(-0.346160695897863,-1.92634582341936,
3.88106121184558));
#17875=CARTESIAN_POINT('Ctrl Pts',(-0.982605239509219,-1.81197794438196,
3.84402395694362));
#17876=CARTESIAN_POINT('Ctrl Pts',(-1.55676792073795,-1.35101841904471,
3.80698670204166));
#17877=CARTESIAN_POINT('Ctrl Pts',(-1.80599304634745,-0.754337176157871,
3.7699494471397));
#17878=CARTESIAN_POINT('Ctrl Pts',(-1.90486450707571,-0.517624501506378,
3.75525619546788));
#17879=CARTESIAN_POINT('Ctrl Pts',(-1.95259626934014,-0.259551514418081,
3.74056294379605));
#17880=CARTESIAN_POINT('Ctrl Pts',(-1.95135083467133,-0.00103713828173369,
3.72586969212423));
#17881=CARTESIAN_POINT('Ctrl Pts',(-1.95121488712599,-0.000926387452031019,
3.62413030787576));
#17882=CARTESIAN_POINT('Ctrl Pts',(-1.95235789806598,-0.268025714432167,
3.63930888231939));
#17883=CARTESIAN_POINT('Ctrl Pts',(-1.90131408798319,-0.534706827138703,
3.65448745676302));
#17884=CARTESIAN_POINT('Ctrl Pts',(-1.79599159513475,-0.777878789707524,
3.66966603120664));
#17885=CARTESIAN_POINT('Ctrl Pts',(-1.53878536027985,-1.37172482603906,
3.7067333648552));
#17886=CARTESIAN_POINT('Ctrl Pts',(-0.95787366592914,-1.82536775021069,
3.74380069850375));
#17887=CARTESIAN_POINT('Ctrl Pts',(-0.319394948990622,-1.93097594180636,
3.7808680321523));
#17888=CARTESIAN_POINT('Ctrl Pts',(0.319083767947896,-2.03658413340203,
3.81793536580085));
#17889=CARTESIAN_POINT('Ctrl Pts',(1.01512950747422,-1.79415759242175,3.85500269944941));
#17890=CARTESIAN_POINT('Ctrl Pts',(1.44985640976405,-1.31476142791748,3.89207003309796));
#17891=CARTESIAN_POINT('Ctrl Pts',(1.88458331205388,-0.835365263413203,
3.92913736674651));
#17892=CARTESIAN_POINT('Ctrl Pts',(2.05799137710721,-0.118999475384943,
3.96620470039506));
#17893=CARTESIAN_POINT('Ctrl Pts',(1.89063556735747,0.506140664950446,4.00327203404361));
#17894=CARTESIAN_POINT('Ctrl Pts',(1.72327975760774,1.13128080528583,4.04033936769217));
#17895=CARTESIAN_POINT('Ctrl Pts',(1.21516007305495,1.66519529792834,4.07740670134072));
#17896=CARTESIAN_POINT('Ctrl Pts',(0.599066075218673,1.86327696781671,4.11447403498927));
#17897=CARTESIAN_POINT('Ctrl Pts',(-0.0170279226176054,2.06135863770508,
4.15154136863782));
#17898=CARTESIAN_POINT('Ctrl Pts',(-0.74109623373737,1.92360748483931,4.18860870228637));
#17899=CARTESIAN_POINT('Ctrl Pts',(-1.24141475891726,1.51313271645821,4.22567603593493));
#17900=CARTESIAN_POINT('Ctrl Pts',(-1.68437887571559,1.14971304660178,4.25849412658187));
#17901=CARTESIAN_POINT('Ctrl Pts',(-1.95195229526599,0.572513574095349,
4.29131221722882));
#17902=CARTESIAN_POINT('Ctrl Pts',(-1.95619906720822,-0.0012405029508829,
4.32413030787576));
#17903=CARTESIAN_POINT('Origin',(0.,0.,0.));
#17904=CARTESIAN_POINT('',(-1.95458379985314,0.00173431571939442,5.12586969212423));
#17905=CARTESIAN_POINT('',(-1.95503514488101,0.00166188402949293,5.02413030787576));
#17906=CARTESIAN_POINT('',(-1.954,-2.39295984553393E-16,0.));
#17907=CARTESIAN_POINT('Ctrl Pts',(-1.95458379985314,0.00173431571939442,
5.12586969212423));
#17908=CARTESIAN_POINT('Ctrl Pts',(-1.95579765110671,0.133598995356774,
5.11834333595291));
#17909=CARTESIAN_POINT('Ctrl Pts',(-1.94359203725346,0.26524025398885,5.1108169797816));
#17910=CARTESIAN_POINT('Ctrl Pts',(-1.9171424819943,0.393954518342425,5.10329062361028));
#17911=CARTESIAN_POINT('Ctrl Pts',(-1.78698402312272,1.02735837405563,5.06625336870832));
#17912=CARTESIAN_POINT('Ctrl Pts',(-1.31188979988961,1.58988121587218,5.02921611380637));
#17913=CARTESIAN_POINT('Ctrl Pts',(-0.709195781064526,1.82419209594539,
4.9921788589044));
#17914=CARTESIAN_POINT('Ctrl Pts',(-0.10650176223944,2.0585029760186,4.95514160400244));
#17915=CARTESIAN_POINT('Ctrl Pts',(0.623792052177624,1.96460189434848,4.91810434910048));
#17916=CARTESIAN_POINT('Ctrl Pts',(1.14760642930858,1.58544471433065,4.88106709419852));
#17917=CARTESIAN_POINT('Ctrl Pts',(1.67142080643954,1.20628753431283,4.84402983929656));
#17918=CARTESIAN_POINT('Ctrl Pts',(1.98875574628439,0.541874255947292,4.8069925843946));
#17919=CARTESIAN_POINT('Ctrl Pts',(1.95444363113096,-0.103853509912194,
4.76995532949264));
#17920=CARTESIAN_POINT('Ctrl Pts',(1.92013151597754,-0.749581275771674,
4.73291807459068));
#17921=CARTESIAN_POINT('Ctrl Pts',(1.53417234582584,-1.3766235291251,4.69588081968872));
#17922=CARTESIAN_POINT('Ctrl Pts',(0.973126487121711,-1.69813435830372,
4.65884356478676));
#17923=CARTESIAN_POINT('Ctrl Pts',(0.412080628417575,-2.01964518748234,
4.62180630988479));
#17924=CARTESIAN_POINT('Ctrl Pts',(-0.324051918839002,-2.03562459248615,
4.58476905498283));
#17925=CARTESIAN_POINT('Ctrl Pts',(-0.898520942843956,-1.73876265604603,
4.54773180008087));
#17926=CARTESIAN_POINT('Ctrl Pts',(-1.47298996684891,-1.44190071960592,
4.51069454517891));
#17927=CARTESIAN_POINT('Ctrl Pts',(-1.88579546760224,-0.832197441721883,
4.47365729027695));
#17928=CARTESIAN_POINT('Ctrl Pts',(-1.94809599212019,-0.188566869504432,
4.43662003537499));
#17929=CARTESIAN_POINT('Ctrl Pts',(-1.95412372487237,-0.126293989613301,
4.43303658762474));
#17930=CARTESIAN_POINT('Ctrl Pts',(-1.95687036296404,-0.0637035146184469,
4.42945313987448));
#17931=CARTESIAN_POINT('Ctrl Pts',(-1.95645531603829,-0.0010761721163155,
4.42586969212423));
#17932=CARTESIAN_POINT('Ctrl Pts',(-1.95619906720822,-0.0012405029508829,
4.32413030787576));
#17933=CARTESIAN_POINT('Ctrl Pts',(-1.95674893362639,-0.0755294225214843,
4.32837955087737));
#17934=CARTESIAN_POINT('Ctrl Pts',(-1.95288420038623,-0.149760580973872,
4.33262879387898));
#17935=CARTESIAN_POINT('Ctrl Pts',(-1.94441398713267,-0.223462453035597,
4.33687803688058));
#17936=CARTESIAN_POINT('Ctrl Pts',(-1.87052595092818,-0.866384470251901,
4.37394537052913));
#17937=CARTESIAN_POINT('Ctrl Pts',(-1.44618113927919,-1.4690301207881,4.41101270417768));
#17938=CARTESIAN_POINT('Ctrl Pts',(-0.86578855785897,-1.75530378976244,
4.44808003782624));
#17939=CARTESIAN_POINT('Ctrl Pts',(-0.285395976438753,-2.04157745873679,
4.48514737147479));
#17940=CARTESIAN_POINT('Ctrl Pts',(0.451044374752689,-2.01147914614929,
4.52221470512334));
#17941=CARTESIAN_POINT('Ctrl Pts',(1.00614027956814,-1.67879806978219,4.55928203877189));
#17942=CARTESIAN_POINT('Ctrl Pts',(1.56123618438359,-1.34611699341509,4.59634937242044));
#17943=CARTESIAN_POINT('Ctrl Pts',(1.93498764282306,-0.710853153268378,
4.633416706069));
#17944=CARTESIAN_POINT('Ctrl Pts',(1.95616444914465,-0.0640458365273947,
4.67048403971755));
#17945=CARTESIAN_POINT('Ctrl Pts',(1.97734125546624,0.582761480213589,4.7075513733661));
#17946=CARTESIAN_POINT('Ctrl Pts',(1.64594340966995,1.24111227354885,4.74461870701465));
#17947=CARTESIAN_POINT('Ctrl Pts',(1.1137972659727,1.60939021731388,4.7816860406632));
#17948=CARTESIAN_POINT('Ctrl Pts',(0.58165112227545,1.97766816107891,4.81875337431176));
#17949=CARTESIAN_POINT('Ctrl Pts',(-0.151243319322761,2.05587325527372,
4.85582070796031));
#17950=CARTESIAN_POINT('Ctrl Pts',(-0.74911836296885,1.80817667818627,4.89288804160886));
#17951=CARTESIAN_POINT('Ctrl Pts',(-1.34699340661495,1.56048010109882,4.92995537525741));
#17952=CARTESIAN_POINT('Ctrl Pts',(-1.80984905230891,0.986881852729116,
4.96702270890596));
#17953=CARTESIAN_POINT('Ctrl Pts',(-1.92563297048424,0.350169793468709,
5.00409004255452));
#17954=CARTESIAN_POINT('Ctrl Pts',(-1.94649896588392,0.235424748484748,
5.01077013099493));
#17955=CARTESIAN_POINT('Ctrl Pts',(-1.95609296160575,0.118629928772321,
5.01745021943535));
#17956=CARTESIAN_POINT('Ctrl Pts',(-1.95503514488101,0.00166188402949293,
5.02413030787576));
#17957=CARTESIAN_POINT('Origin',(0.,0.,0.));
#17958=CARTESIAN_POINT('',(-1.95079798926752,-3.39345409606611E-5,5.82586969212423));
#17959=CARTESIAN_POINT('',(-1.95081926285686,0.000266806291091909,5.72413030787576));
#17960=CARTESIAN_POINT('',(-1.954,-2.39295984553393E-16,0.));
#17961=CARTESIAN_POINT('Ctrl Pts',(-1.95079827866809,-3.39314739267183E-5,
5.82586969212423));
#17962=CARTESIAN_POINT('Ctrl Pts',(-1.95074743468102,0.328084477385078,
5.80723353203135));
#17963=CARTESIAN_POINT('Ctrl Pts',(-1.87239681557632,0.656225698195148,
5.78859737193847));
#17964=CARTESIAN_POINT('Ctrl Pts',(-1.71588222891389,0.941479492766077,
5.76996121184558));
#17965=CARTESIAN_POINT('Ctrl Pts',(-1.4048272361901,1.50838906258186,5.73292395694362));
#17966=CARTESIAN_POINT('Ctrl Pts',(-0.785047590103655,1.90590592866216,
5.69588670204165));
#17967=CARTESIAN_POINT('Ctrl Pts',(-0.140066859714564,1.95218255642174,
5.65884944713969));
#17968=CARTESIAN_POINT('Ctrl Pts',(0.504913870674523,1.99845918418131,5.62181219223773));
#17969=CARTESIAN_POINT('Ctrl Pts',(1.17509568536624,1.69349557362016,5.58477493733578));
#17970=CARTESIAN_POINT('Ctrl Pts',(1.5638981065899,1.17679997067967,5.54773768243382));
#17971=CARTESIAN_POINT('Ctrl Pts',(1.95270052781355,0.660104367739175,5.51070042753186));
#17972=CARTESIAN_POINT('Ctrl Pts',(2.06012355556913,-0.0683232275806662,
5.47366317262989));
#17973=CARTESIAN_POINT('Ctrl Pts',(1.83702559506323,-0.675257300496502,
5.43662591772793));
#17974=CARTESIAN_POINT('Ctrl Pts',(1.61392763455733,-1.28219137341235,5.39958866282597));
#17975=CARTESIAN_POINT('Ctrl Pts',(1.06030868578995,-1.76763192392419,5.36255140792401));
#17976=CARTESIAN_POINT('Ctrl Pts',(0.429426533588159,-1.90950996620586,
5.32551415302205));
#17977=CARTESIAN_POINT('Ctrl Pts',(-0.201455618613625,-2.05138800848752,
5.28847689812009));
#17978=CARTESIAN_POINT('Ctrl Pts',(-0.909600974249807,-1.84970354253902,
5.25143964321813));
#17979=CARTESIAN_POINT('Ctrl Pts',(-1.37106230481287,-1.39671887475983,
5.21440238831617));
#17980=CARTESIAN_POINT('Ctrl Pts',(-1.73874988399236,-1.03578541214894,
5.18489148958552));
#17981=CARTESIAN_POINT('Ctrl Pts',(-1.94982428002672,-0.515308077485324,
5.15538059085487));
#17982=CARTESIAN_POINT('Ctrl Pts',(-1.95458379985314,0.00173431571939442,
5.12586969212423));
#17983=CARTESIAN_POINT('Ctrl Pts',(-1.95503514488101,0.00166188402949293,
5.02413030787576));
#17984=CARTESIAN_POINT('Ctrl Pts',(-1.95022321215187,-0.530417397378261,
5.0545175530839));
#17985=CARTESIAN_POINT('Ctrl Pts',(-1.72499597458382,-1.06608118124287,
5.08490479829204));
#17986=CARTESIAN_POINT('Ctrl Pts',(-1.33773156155863,-1.42869013102344,
5.11529204350017));
#17987=CARTESIAN_POINT('Ctrl Pts',(-0.86533404380103,-1.87101212610407,
5.15235937714873));
#17988=CARTESIAN_POINT('Ctrl Pts',(-0.151826817629148,-2.05583024611426,
5.18942671079728));
#17989=CARTESIAN_POINT('Ctrl Pts',(0.475904465069911,-1.8984720596839,5.22649404444583));
#17990=CARTESIAN_POINT('Ctrl Pts',(1.10363574776897,-1.74111387325355,5.26356137809438));
#17991=CARTESIAN_POINT('Ctrl Pts',(1.6455910869952,-1.24157938038265,5.30062871174293));
#17992=CARTESIAN_POINT('Ctrl Pts',(1.85347948041758,-0.628724929476167,
5.33769604539148));
#17993=CARTESIAN_POINT('Ctrl Pts',(2.06136787383997,-0.015870478569668,
5.37476337904004));
#17994=CARTESIAN_POINT('Ctrl Pts',(1.93518932145849,0.710303930372423,5.41183071268859));
#17995=CARTESIAN_POINT('Ctrl Pts',(1.53275116822559,1.21710931209029,5.44889804633714));
#17996=CARTESIAN_POINT('Ctrl Pts',(1.13031301499269,1.72391469380815,5.48596537998569));
#17997=CARTESIAN_POINT('Ctrl Pts',(0.451615260908389,2.01135104830178,5.52303271363424));
#17998=CARTESIAN_POINT('Ctrl Pts',(-0.192404026912741,1.94773250517156,
5.56010004728279));
#17999=CARTESIAN_POINT('Ctrl Pts',(-0.836423314733875,1.88411396204135,
5.59716738093134));
#18000=CARTESIAN_POINT('Ctrl Pts',(-1.44576413629184,1.46944052128728,5.6342347145799));
#18001=CARTESIAN_POINT('Ctrl Pts',(-1.74126355620191,0.893690354158911,
5.67130204822845));
#18002=CARTESIAN_POINT('Ctrl Pts',(-1.88164520354535,0.620171181280857,
5.68891146811089));
#18003=CARTESIAN_POINT('Ctrl Pts',(-1.95119678622385,0.310299013274676,
5.70652088799333));
#18004=CARTESIAN_POINT('Ctrl Pts',(-1.95081926285686,0.000266806291091909,
5.72413030787576));
#18005=CARTESIAN_POINT('Origin',(0.,0.,0.));
#18006=CARTESIAN_POINT('',(-1.95470825951396,-0.00171604386803359,6.52586969212423));
#18007=CARTESIAN_POINT('',(-1.954054516794,-0.00178804188155213,6.42413030787577));
#18008=CARTESIAN_POINT('',(-1.954,-2.39295984553393E-16,0.));
#18009=CARTESIAN_POINT('Ctrl Pts',(-1.95470825951396,-0.00171604386803359,
6.52586969212423));
#18010=CARTESIAN_POINT('Ctrl Pts',(-1.94992854745838,0.51935938865238,6.49612372810978));
#18011=CARTESIAN_POINT('Ctrl Pts',(-1.73510566406059,1.04391419457857,6.46637776409532));
#18012=CARTESIAN_POINT('Ctrl Pts',(-1.36219391366738,1.40536941793186,6.43663180008087));
#18013=CARTESIAN_POINT('Ctrl Pts',(-0.897874534119316,1.85542406186529,
6.39959454517891));
#18014=CARTESIAN_POINT('Ctrl Pts',(-0.188466746172986,2.05262208241376,
6.36255729027695));
#18015=CARTESIAN_POINT('Ctrl Pts',(0.441504710548841,1.90675353660593,6.32552003537499));
#18016=CARTESIAN_POINT('Ctrl Pts',(1.07147616727065,1.76088499079811,6.28848278047303));
#18017=CARTESIAN_POINT('Ctrl Pts',(1.62201129276796,1.27194987863399,6.25144552557107));
#18018=CARTESIAN_POINT('Ctrl Pts',(1.84126302416029,0.663615803388951,6.21440827066911));
#18019=CARTESIAN_POINT('Ctrl Pts',(2.06051475555262,0.0552817281439051,
6.17737101576715));
#18020=CARTESIAN_POINT('Ctrl Pts',(1.94848309283996,-0.672451310182071,
6.14033376086519));
#18021=CARTESIAN_POINT('Ctrl Pts',(1.55641789066206,-1.18667552789108,6.10329650596323));
#18022=CARTESIAN_POINT('Ctrl Pts',(1.16435268848415,-1.7008997456001,6.06625925106126));
#18023=CARTESIAN_POINT('Ctrl Pts',(0.492253946840989,-2.00161514269215,
6.02922199615931));
#18024=CARTESIAN_POINT('Ctrl Pts',(-0.152420941573553,-1.95125685529952,
5.99218474125735));
#18025=CARTESIAN_POINT('Ctrl Pts',(-0.79709582998809,-1.90089856790688,
5.95514748635538));
#18026=CARTESIAN_POINT('Ctrl Pts',(-1.41434686517401,-1.49946659602955,
5.91811023145342));
#18027=CARTESIAN_POINT('Ctrl Pts',(-1.7218072130864,-0.930599473315251,
5.88107297655146));
#18028=CARTESIAN_POINT('Ctrl Pts',(-1.8745617038537,-0.647971133646427,
5.86267188174238));
#18029=CARTESIAN_POINT('Ctrl Pts',(-1.95084848133978,-0.324013652614182,
5.84427078693331));
#18030=CARTESIAN_POINT('Ctrl Pts',(-1.95079827866809,-3.39314739267183E-5,
5.82586969212423));
#18031=CARTESIAN_POINT('Ctrl Pts',(-1.95081926285686,0.000266806291091909,
5.72413030787576));
#18032=CARTESIAN_POINT('Ctrl Pts',(-1.95040211015287,-0.342310063843146,
5.74358822164188));
#18033=CARTESIAN_POINT('Ctrl Pts',(-1.86460411668041,-0.685082335623694,
5.76304613540799));
#18034=CARTESIAN_POINT('Ctrl Pts',(-1.69464079239607,-0.979221020005547,
5.78250404917411));
#18035=CARTESIAN_POINT('Ctrl Pts',(-1.37086059041801,-1.53955533353895,
5.81957138282266));
#18036=CARTESIAN_POINT('Ctrl Pts',(-0.741642168199709,-1.92339706710309,
5.85663871647121));
#18037=CARTESIAN_POINT('Ctrl Pts',(-0.0952551698061251,-1.95489326406863,
5.89370605011977));
#18038=CARTESIAN_POINT('Ctrl Pts',(0.551131828587468,-1.98638946103417,
5.93077338376832));
#18039=CARTESIAN_POINT('Ctrl Pts',(1.21468740315634,-1.6655401214011,5.96784071741687));
#18040=CARTESIAN_POINT('Ctrl Pts',(1.59141071326467,-1.1393389148879,6.00490805106542));
#18041=CARTESIAN_POINT('Ctrl Pts',(1.96813402337299,-0.613137708374708,
6.04197538471397));
#18042=CARTESIAN_POINT('Ctrl Pts',(2.05802506902077,0.118415365018621,6.07904271836252));
#18043=CARTESIAN_POINT('Ctrl Pts',(1.81990123568346,0.720167142842566,6.11611005201108));
#18044=CARTESIAN_POINT('Ctrl Pts',(1.58177740234616,1.32191892066651,6.15317738565963));
#18045=CARTESIAN_POINT('Ctrl Pts',(1.01563869002379,1.79386940292107,6.19024471930818));
#18046=CARTESIAN_POINT('Ctrl Pts',(0.380855453001195,1.91979955860115,6.22731205295673));
#18047=CARTESIAN_POINT('Ctrl Pts',(-0.253927784021398,2.04572971428122,
6.26437938660528));
#18048=CARTESIAN_POINT('Ctrl Pts',(-0.957355545744209,1.82563954338681,
6.30144672025383));
#18049=CARTESIAN_POINT('Ctrl Pts',(-1.40715997837402,1.36036098757553,6.33851405390239));
#18050=CARTESIAN_POINT('Ctrl Pts',(-1.75347182721572,1.0021353561665,6.36705280522685));
#18051=CARTESIAN_POINT('Ctrl Pts',(-1.94944302076728,0.498569063116626,
6.39559155655131));
#18052=CARTESIAN_POINT('Ctrl Pts',(-1.954054516794,-0.00178804188155213,
6.42413030787577));
#18053=CARTESIAN_POINT('Origin',(0.,0.,0.));
#18054=CARTESIAN_POINT('',(-1.95636485901942,0.00113456228253272,7.22586969212423));
#18055=CARTESIAN_POINT('',(-1.95685604123946,0.000756211846537467,7.12413030787577));
#18056=CARTESIAN_POINT('',(-1.954,-2.39295984553393E-16,0.));
#18057=CARTESIAN_POINT('Ctrl Pts',(-1.95636485901942,0.00113456228253272,
7.22586969212423));
#18058=CARTESIAN_POINT('Ctrl Pts',(-1.95682612605948,0.0678782264229027,
7.22205117909017));
#18059=CARTESIAN_POINT('Ctrl Pts',(-1.95370640484,0.134578270129128,7.21823266605611));
#18060=CARTESIAN_POINT('Ctrl Pts',(-1.94686336470326,0.200894109800786,
7.21441415302205));
#18061=CARTESIAN_POINT('Ctrl Pts',(-1.88049003571683,0.844117436799507,
7.17737689812009));
#18062=CARTESIAN_POINT('Ctrl Pts',(-1.46383354330961,1.45119553755835,7.14033964321813));
#18063=CARTESIAN_POINT('Ctrl Pts',(-0.887496963111741,1.7444152651618,7.10330238831617));
#18064=CARTESIAN_POINT('Ctrl Pts',(-0.311160382913887,2.03763499276525,
7.0662651334142));
#18065=CARTESIAN_POINT('Ctrl Pts',(0.42485628507463,2.01699634721332,7.02922787851224));
#18066=CARTESIAN_POINT('Ctrl Pts',(0.983855814420553,1.6919406608931,6.99219062361028));
#18067=CARTESIAN_POINT('Ctrl Pts',(1.5428553437665,1.36688497457287,6.95515336870832));
#18068=CARTESIAN_POINT('Ctrl Pts',(1.92483773446985,0.737412247484355,6.91811611380636));
#18069=CARTESIAN_POINT('Ctrl Pts',(1.95506184522045,0.0914802298548023,
6.8810788589044));
#18070=CARTESIAN_POINT('Ctrl Pts',(1.98528595597105,-0.554451787774746,
6.84404160400244));
#18071=CARTESIAN_POINT('Ctrl Pts',(1.66375178676889,-1.21684309594531,6.80700434910048));
#18072=CARTESIAN_POINT('Ctrl Pts',(1.13754792239338,-1.59267705016464,6.76996709419852));
#18073=CARTESIAN_POINT('Ctrl Pts',(0.611344058017871,-1.96851100438396,
6.73292983929656));
#18074=CARTESIAN_POINT('Ctrl Pts',(-0.119529501530993,-2.05778760465205,
6.69589258439459));
#18075=CARTESIAN_POINT('Ctrl Pts',(-0.72072831037795,-1.81966649740579,
6.65885532949263));
#18076=CARTESIAN_POINT('Ctrl Pts',(-1.3219271192249,-1.58154539015953,6.62181807459067));
#18077=CARTESIAN_POINT('Ctrl Pts',(-1.79345117736996,-1.01602657539894,
6.58478081968872));
#18078=CARTESIAN_POINT('Ctrl Pts',(-1.91959772086759,-0.381811534359454,
6.54774356478676));
#18079=CARTESIAN_POINT('Ctrl Pts',(-1.94443139565072,-0.256957617359055,
6.54045227389925));
#18080=CARTESIAN_POINT('Ctrl Pts',(-1.95587985613591,-0.129441356485054,
6.53316098301174));
#18081=CARTESIAN_POINT('Ctrl Pts',(-1.95470825951396,-0.00171604386803359,
6.52586969212423));
#18082=CARTESIAN_POINT('Ctrl Pts',(-1.954054516794,-0.00178804188155213,
6.42413030787577));
#18083=CARTESIAN_POINT('Ctrl Pts',(-1.95543262626536,-0.151315844023487,
6.43265889019986));
#18084=CARTESIAN_POINT('Ctrl Pts',(-1.93972104383109,-0.300557044358562,
6.44118747252395));
#18085=CARTESIAN_POINT('Ctrl Pts',(-1.90582502907504,-0.445547056796695,
6.44971605484804));
#18086=CARTESIAN_POINT('Ctrl Pts',(-1.75850454360942,-1.07570960462949,
6.4867833884966));
#18087=CARTESIAN_POINT('Ctrl Pts',(-1.26768246914137,-1.62556775956693,
6.52385072214515));
#18088=CARTESIAN_POINT('Ctrl Pts',(-0.658223653418358,-1.84320992928983,
6.5609180557937));
#18089=CARTESIAN_POINT('Ctrl Pts',(-0.0487648376953535,-2.06085209901273,
6.59798538944225));
#18090=CARTESIAN_POINT('Ctrl Pts',(0.679330719282597,-1.94627828352109,
6.63505272309081));
#18091=CARTESIAN_POINT('Ctrl Pts',(1.19249387898998,-1.55197924267736,6.67212005673936));
#18092=CARTESIAN_POINT('Ctrl Pts',(1.70565703869737,-1.15768020183362,6.70918739038791));
#18093=CARTESIAN_POINT('Ctrl Pts',(2.00388780113418,-0.483655935637787,
6.74625472403646));
#18094=CARTESIAN_POINT('Ctrl Pts',(1.95055495411266,0.161296597217467,6.78332205768501));
#18095=CARTESIAN_POINT('Ctrl Pts',(1.89722210709115,0.806249130072731,6.82038939133356));
#18096=CARTESIAN_POINT('Ctrl Pts',(1.49232565061129,1.42212992958742,6.85745672498212));
#18097=CARTESIAN_POINT('Ctrl Pts',(0.921364535931439,1.72677983938191,6.89452405863067));
#18098=CARTESIAN_POINT('Ctrl Pts',(0.35040342125159,2.03142974917639,6.93159139227922));
#18099=CARTESIAN_POINT('Ctrl Pts',(-0.386622351628245,2.02484876925069,
6.96865872592777));
#18100=CARTESIAN_POINT('Ctrl Pts',(-0.95205236204405,1.7100519056834,7.00572605957632));
#18101=CARTESIAN_POINT('Ctrl Pts',(-1.51748237245986,1.39525504211611,7.04279339322487));
#18102=CARTESIAN_POINT('Ctrl Pts',(-1.91131662041163,0.772242294907221,
7.07986072687343));
#18103=CARTESIAN_POINT('Ctrl Pts',(-1.95312418617604,0.126440243047374,
7.11692806052198));
#18104=CARTESIAN_POINT('Ctrl Pts',(-1.95583194707364,0.0846134226707359,
7.11932880963991));
#18105=CARTESIAN_POINT('Ctrl Pts',(-1.95706302779737,0.0426910058065101,
7.12172955875784));
#18106=CARTESIAN_POINT('Ctrl Pts',(-1.95685604123946,0.000756211846537467,
7.12413030787577));
#18107=CARTESIAN_POINT('Origin',(0.,0.,0.));
#18108=CARTESIAN_POINT('',(-1.95128693461656,0.000980964721550987,7.92586969212423));
#18109=CARTESIAN_POINT('',(-1.95179084094767,0.00133979406531506,7.82413030787577));
#18110=CARTESIAN_POINT('',(-1.954,-2.39295984553393E-16,0.));
#18111=CARTESIAN_POINT('Ctrl Pts',(-1.95128693461656,0.000980964721550987,
7.92586969212423));
#18112=CARTESIAN_POINT('Ctrl Pts',(-1.95248078249778,0.263652730728045,
7.9109413751686));
#18113=CARTESIAN_POINT('Ctrl Pts',(-1.90315517629326,0.525894534188289,
7.89601305821297));
#18114=CARTESIAN_POINT('Ctrl Pts',(-1.80118142285547,0.765753467326086,
7.88108474125734));
#18115=CARTESIAN_POINT('Ctrl Pts',(-1.54818385383207,1.36084509577563,7.84404748635538));
#18116=CARTESIAN_POINT('Ctrl Pts',(-0.971116173277759,1.81816132921196,
7.80701023145342));
#18117=CARTESIAN_POINT('Ctrl Pts',(-0.333960757905731,1.9284984258719,7.76997297655146));
#18118=CARTESIAN_POINT('Ctrl Pts',(0.303194657466307,2.03883552253184,7.7329357216495));
#18119=CARTESIAN_POINT('Ctrl Pts',(1.00043780765606,1.80219348241539,7.69589846674754));
#18120=CARTESIAN_POINT('Ctrl Pts',(1.43880759949705,1.3268265031207,7.65886121184558));
#18121=CARTESIAN_POINT('Ctrl Pts',(1.87717739133805,0.851459523826022,7.62182395694362));
#18122=CARTESIAN_POINT('Ctrl Pts',(2.05667382483028,0.137367605353111,7.58478670204165));
#18123=CARTESIAN_POINT('Ctrl Pts',(1.8951853172685,-0.488781846291726,7.54774944713969));
#18124=CARTESIAN_POINT('Ctrl Pts',(1.73369680970672,-1.11493129793655,7.51071219223773));
#18125=CARTESIAN_POINT('Ctrl Pts',(1.23122336109093,-1.65313828275331,7.47367493733578));
#18126=CARTESIAN_POINT('Ctrl Pts',(0.617625480567028,-1.85719528451254,
7.43663768243382));
#18127=CARTESIAN_POINT('Ctrl Pts',(0.00402760004311595,-2.06125228627176,
7.39960042753186));
#18128=CARTESIAN_POINT('Ctrl Pts',(-0.720694712388916,-1.93115930497345,
7.36256317262989));
#18129=CARTESIAN_POINT('Ctrl Pts',(-1.22501078582212,-1.52642853770499,
7.32552591772793));
#18130=CARTESIAN_POINT('Ctrl Pts',(-1.67733225261428,-1.16342520715373,
7.29230717586003));
#18131=CARTESIAN_POINT('Ctrl Pts',(-1.95235211620587,-0.579494737819326,
7.25908843399213));
#18132=CARTESIAN_POINT('Ctrl Pts',(-1.95636485901942,0.00113456228253272,
7.22586969212423));
#18133=CARTESIAN_POINT('Ctrl Pts',(-1.95685604123946,0.000756211846537467,
7.12413030787577));
#18134=CARTESIAN_POINT('Ctrl Pts',(-1.95386717540877,-0.604778147712892,
7.15879689240639));
#18135=CARTESIAN_POINT('Ctrl Pts',(-1.65102574974132,-1.21289326541241,
7.19346347693701));
#18136=CARTESIAN_POINT('Ctrl Pts',(-1.16459038479062,-1.57302589296855,
7.22813006146763));
#18137=CARTESIAN_POINT('Ctrl Pts',(-0.644468134063717,-1.95809862061383,
7.26519739511619));
#18138=CARTESIAN_POINT('Ctrl Pts',(0.0855572509671633,-2.05965271939359,
7.30226472876474));
#18139=CARTESIAN_POINT('Ctrl Pts',(0.691032502683693,-1.83116227947434,
7.33933206241329));
#18140=CARTESIAN_POINT('Ctrl Pts',(1.29650775440023,-1.60267183955508,7.37639939606184));
#18141=CARTESIAN_POINT('Ctrl Pts',(1.7774328728024,-1.0441368609368,7.41346672971039));
#18142=CARTESIAN_POINT('Ctrl Pts',(1.91347719234508,-0.411444116083022,
7.45053406335894));
#18143=CARTESIAN_POINT('Ctrl Pts',(2.04952151188775,0.221248628770744,7.4876013970075));
#18144=CARTESIAN_POINT('Ctrl Pts',(1.84068503257092,0.928099139860014,7.52466873065605));
#18145=CARTESIAN_POINT('Ctrl Pts',(1.38264394156525,1.38527144266209,7.5617360643046));
#18146=CARTESIAN_POINT('Ctrl Pts',(0.924602850559573,1.84244374546417,7.59880339795316));
#18147=CARTESIAN_POINT('Ctrl Pts',(0.21735714786506,2.04993783997907,7.63587073160171));
#18148=CARTESIAN_POINT('Ctrl Pts',(-0.415076170159516,1.9126925888594,7.67293806525026));
#18149=CARTESIAN_POINT('Ctrl Pts',(-1.0475094881841,1.77544733773972,7.71000539889881));
#18150=CARTESIAN_POINT('Ctrl Pts',(-1.60513042153874,1.29346274098546,7.74707273254736));
#18151=CARTESIAN_POINT('Ctrl Pts',(-1.83247093326142,0.687554760545781,
7.78414006619591));
#18152=CARTESIAN_POINT('Ctrl Pts',(-1.91422667443603,0.469659341691089,
7.79747014675586));
#18153=CARTESIAN_POINT('Ctrl Pts',(-1.95326886402229,0.235737517711039,
7.81080022731581));
#18154=CARTESIAN_POINT('Ctrl Pts',(-1.95179084094767,0.00133979406531506,
7.82413030787577));
#18155=CARTESIAN_POINT('Origin',(0.,0.,0.));
#18156=CARTESIAN_POINT('',(-1.95285709583883,-0.00166548583676096,8.62586969212423));
#18157=CARTESIAN_POINT('',(-1.95199070173634,-0.00143915622514865,8.52413030787577));
#18158=CARTESIAN_POINT('',(-1.954,-2.39295984553393E-16,0.));
#18159=CARTESIAN_POINT('Ctrl Pts',(-1.95285709583883,-0.00166548583676096,
8.62586969212423));
#18160=CARTESIAN_POINT('Ctrl Pts',(-1.94908690947408,0.455599167126523,
8.59983157124703));
#18161=CARTESIAN_POINT('Ctrl Pts',(-1.78874742560419,0.915224010975134,
8.57379345036984));
#18162=CARTESIAN_POINT('Ctrl Pts',(-1.49546401894218,1.26258187482945,8.54775532949264));
#18163=CARTESIAN_POINT('Ctrl Pts',(-1.07829058533359,1.75667212836379,8.51071807459068));
#18164=CARTESIAN_POINT('Ctrl Pts',(-0.392132937906689,2.02361363589085,
8.47368081968872));
#18165=CARTESIAN_POINT('Ctrl Pts',(0.249226660225596,1.94126935410646,8.43664356478675));
#18166=CARTESIAN_POINT('Ctrl Pts',(0.890586258357889,1.85892507232208,8.39960630988479));
#18167=CARTESIAN_POINT('Ctrl Pts',(1.48714780719556,1.42729500122627,8.36256905498283));
#18168=CARTESIAN_POINT('Ctrl Pts',(1.76595313409068,0.84384378564397,8.32553180008087));
#18169=CARTESIAN_POINT('Ctrl Pts',(2.04475846098579,0.260392570061681,8.28849454517891));
#18170=CARTESIAN_POINT('Ctrl Pts',(2.00580756593834,-0.474879790007082,
8.25145729027695));
#18171=CARTESIAN_POINT('Ctrl Pts',(1.66694824118237,-1.02562274217559,8.21442003537499));
#18172=CARTESIAN_POINT('Ctrl Pts',(1.3280889164264,-1.5763656943441,8.17738278047303));
#18173=CARTESIAN_POINT('Ctrl Pts',(0.689321161961899,-1.94257923861236,
8.14034552557107));
#18174=CARTESIAN_POINT('Ctrl Pts',(0.0428393990027941,-1.95673258160789,
8.10330827066911));
#18175=CARTESIAN_POINT('Ctrl Pts',(-0.60364236395632,-1.97088592460343,
8.06627101576715));
#18176=CARTESIAN_POINT('Ctrl Pts',(-1.25783813541006,-1.63297906632622,
8.02923376086519));
#18177=CARTESIAN_POINT('Ctrl Pts',(-1.62047229239069,-1.09759212545623,
7.99219650596323));
#18178=CARTESIAN_POINT('Ctrl Pts',(-1.83694233303294,-0.777999415783143,
7.9700875680169));
#18179=CARTESIAN_POINT('Ctrl Pts',(-1.94951883786448,-0.388037689702213,
7.94797863007056));
#18180=CARTESIAN_POINT('Ctrl Pts',(-1.95128693461656,0.000980964721550987,
7.92586969212423));
#18181=CARTESIAN_POINT('Ctrl Pts',(-1.95179084094767,0.00133979406531506,
7.82413030787577));
#18182=CARTESIAN_POINT('Ctrl Pts',(-1.94915888327607,-0.416058890402282,
7.84786756096437));
#18183=CARTESIAN_POINT('Ctrl Pts',(-1.81803758852289,-0.834966649688199,
7.87160481405297));
#18184=CARTESIAN_POINT('Ctrl Pts',(-1.57081203637628,-1.16757477949376,
7.89534206714157));
#18185=CARTESIAN_POINT('Ctrl Pts',(-1.18475253767773,-1.68696497496857,
7.93240940079012));
#18186=CARTESIAN_POINT('Ctrl Pts',(-0.5155734501899,-1.99591400179311,7.96947673443867));
#18187=CARTESIAN_POINT('Ctrl Pts',(0.130148074857978,-1.95288051881755,
8.00654406808722));
#18188=CARTESIAN_POINT('Ctrl Pts',(0.775869599905848,-1.90984703584199,
8.04361140173578));
#18189=CARTESIAN_POINT('Ctrl Pts',(1.39813356251376,-1.51483104306634,8.08067873538433));
#18190=CARTESIAN_POINT('Ctrl Pts',(1.71185635075732,-0.948804238199317,
8.11774606903288));
#18191=CARTESIAN_POINT('Ctrl Pts',(2.02557913900088,-0.382777433332289,
8.15481340268144));
#18192=CARTESIAN_POINT('Ctrl Pts',(2.03076075288008,0.354260183626113,8.19188073632998));
#18193=CARTESIAN_POINT('Ctrl Pts',(1.72502744155934,0.924641574518184,8.22894806997854));
#18194=CARTESIAN_POINT('Ctrl Pts',(1.41929413023861,1.49502296541025,8.26601540362709));
#18195=CARTESIAN_POINT('Ctrl Pts',(0.80264589371795,1.89874813023598,8.30308273727564));
#18196=CARTESIAN_POINT('Ctrl Pts',(0.157593195636322,1.9508570009308,8.3401500709242));
#18197=CARTESIAN_POINT('Ctrl Pts',(-0.487459502445315,2.00296587162561,
8.37721740457275));
#18198=CARTESIAN_POINT('Ctrl Pts',(-1.16091666208792,1.7034584481895,8.4142847382213));
#18199=CARTESIAN_POINT('Ctrl Pts',(-1.55424059489758,1.18954651103718,8.45135207186985));
#18200=CARTESIAN_POINT('Ctrl Pts',(-1.81165882267556,0.853207201220195,
8.47561148387182));
#18201=CARTESIAN_POINT('Ctrl Pts',(-1.94908776418844,0.42503214287857,8.4998708958738));
#18202=CARTESIAN_POINT('Ctrl Pts',(-1.95199070173634,-0.00143915622514865,
8.52413030787577));
#18203=CARTESIAN_POINT('Origin',(0.,0.,-1.2940562256037));
#18204=CARTESIAN_POINT('',(-1.55459018043874,-0.0013258255983764,8.8559437743963));
#18205=CARTESIAN_POINT('',(-1.55786620250461,-0.000579511545185651,8.99405622560371));
#18206=CARTESIAN_POINT('',(-1.5555,-1.46451138874614E-13,-1.2940562256037));
#18207=CARTESIAN_POINT('',(-0.840025297123077,1.30917445368953,9.44449999999999));
#18208=CARTESIAN_POINT('Ctrl Pts',(-1.55459018043874,-0.00132582559837632,
8.8559437743963));
#18209=CARTESIAN_POINT('Ctrl Pts',(-1.55585799906995,-0.155092401130408,
8.86694290842106));
#18210=CARTESIAN_POINT('Ctrl Pts',(-1.46426308580118,-0.825171155750169,
8.91497929734778));
#18211=CARTESIAN_POINT('Ctrl Pts',(-0.502885372776985,-1.76823019847661,
9.00005294117646));
#18212=CARTESIAN_POINT('Ctrl Pts',(1.21162302759592,-1.38188780683742,9.11116470588235));
#18213=CARTESIAN_POINT('Ctrl Pts',(1.81992793219366,0.268272986849182,9.22227647058824));
#18214=CARTESIAN_POINT('Ctrl Pts',(0.758516013178858,1.6740067592164,9.33338823529411));
#18215=CARTESIAN_POINT('Ctrl Pts',(-0.404795980777633,1.58843718658925,
9.40746274509804));
#18216=CARTESIAN_POINT('Ctrl Pts',(-0.840025297123196,1.30917445368946,
9.4445));
#18217=CARTESIAN_POINT('',(0.964986447796937,1.21999237930745,9.44449999999999));
#18218=CARTESIAN_POINT('Origin',(0.,0.,9.4445));
#18219=CARTESIAN_POINT('Ctrl Pts',(-1.55786620250461,-0.000579511545185591,
8.99405622560371));
#18220=CARTESIAN_POINT('Ctrl Pts',(-1.55797190598053,-0.026693910339596,
8.99593481580826));
#18221=CARTESIAN_POINT('Ctrl Pts',(-1.54554514373521,-0.567968451132823,
9.03488073966137));
#18222=CARTESIAN_POINT('Ctrl Pts',(-0.917075781704608,-1.59325581253419,
9.11089399716304));
#18223=CARTESIAN_POINT('Ctrl Pts',(0.84291969341562,-1.63568507599433,9.22209599810868));
#18224=CARTESIAN_POINT('Ctrl Pts',(1.83002015964776,-0.174643446395858,
9.33329799905435));
#18225=CARTESIAN_POINT('Ctrl Pts',(1.37089695500413,0.898926325849287,9.40743266635145));
#18226=CARTESIAN_POINT('Ctrl Pts',(0.964986447796868,1.2199923793075,9.4445));
#18227=CARTESIAN_POINT('Origin',(0.,0.,-1.2940562256037));
#18228=CARTESIAN_POINT('',(-1.55334023889256,0.000780906153647187,8.1559437743963));
#18229=CARTESIAN_POINT('',(-1.55390047929932,-0.00114565379145046,8.29405622560371));
#18230=CARTESIAN_POINT('',(-1.5555,-1.46451138874614E-13,-1.2940562256037));
#18231=CARTESIAN_POINT('Ctrl Pts',(-1.55334023889256,0.000780906153647377,
8.1559437743963));
#18232=CARTESIAN_POINT('Ctrl Pts',(-1.55193272891411,-0.308901037017355,
8.17805271234263));
#18233=CARTESIAN_POINT('Ctrl Pts',(-1.31218630866396,-1.13937563740009,
8.23719890519093));
#18234=CARTESIAN_POINT('Ctrl Pts',(0.0402435134914415,-1.83793611758998,
8.33338235294118));
#18235=CARTESIAN_POINT('Ctrl Pts',(1.56573467327064,-0.963352952631984,
8.44449411764705));
#18236=CARTESIAN_POINT('Ctrl Pts',(1.65875634765081,0.792608392434986,8.55560588235294));
#18237=CARTESIAN_POINT('Ctrl Pts',(0.234061123673802,1.82341787389281,8.66671764705882));
#18238=CARTESIAN_POINT('Ctrl Pts',(-1.24239126631522,1.24902155512614,8.76683027773994));
#18239=CARTESIAN_POINT('Ctrl Pts',(-1.55158888827378,0.362683983861408,
8.8299056535191));
#18240=CARTESIAN_POINT('Ctrl Pts',(-1.55459018043874,-0.00132582559837632,
8.8559437743963));
#18241=CARTESIAN_POINT('Ctrl Pts',(-1.55390047929932,-0.00114565379145014,
8.29405622560371));
#18242=CARTESIAN_POINT('Ctrl Pts',(-1.55512054028755,-0.180385126241298,
8.30686414725028));
#18243=CARTESIAN_POINT('Ctrl Pts',(-1.44363174688106,-0.876888376361596,
8.35673940254541));
#18244=CARTESIAN_POINT('Ctrl Pts',(-0.415210463238687,-1.79137506804378,
8.4436819914891));
#18245=CARTESIAN_POINT('Ctrl Pts',(1.28062367350908,-1.31967978545922,8.55488399243474));
#18246=CARTESIAN_POINT('Ctrl Pts',(1.80303816946195,0.361303122856545,8.66608599338042));
#18247=CARTESIAN_POINT('Ctrl Pts',(0.673390003682997,1.71105376251155,8.77728799432605));
#18248=CARTESIAN_POINT('Ctrl Pts',(-1.04380561312476,1.49701963955364,8.88661140506718));
#18249=CARTESIAN_POINT('Ctrl Pts',(-1.55588622172637,0.488581390679574,
8.95886748215971));
#18250=CARTESIAN_POINT('Ctrl Pts',(-1.55786620250461,-0.000579511545185591,
8.99405622560371));
#18251=CARTESIAN_POINT('Origin',(0.,0.,-1.2940562256037));
#18252=CARTESIAN_POINT('',(-1.55738256817027,0.00090317893057067,7.4559437743963));
#18253=CARTESIAN_POINT('',(-1.55374137824673,0.00106655561326607,7.59405622560371));
#18254=CARTESIAN_POINT('',(-1.5555,-1.46451138874614E-13,-1.2940562256037));
#18255=CARTESIAN_POINT('Ctrl Pts',(-1.55738256817027,0.000903178930570731,
7.4559437743963));
#18256=CARTESIAN_POINT('Ctrl Pts',(-1.55418818667256,-0.461312213243642,
7.4891625162642));
#18257=CARTESIAN_POINT('Ctrl Pts',(-1.09115753827425,-1.44443285152936,
7.55941851303406));
#18258=CARTESIAN_POINT('Ctrl Pts',(0.580128192863429,-1.74444092308354,
7.66671176470588));
#18259=CARTESIAN_POINT('Ctrl Pts',(1.7801242767762,-0.459106790715335,7.77782352941176));
#18260=CARTESIAN_POINT('Ctrl Pts',(1.35145482596167,1.2462718876643,7.88893529411764));
#18261=CARTESIAN_POINT('Ctrl Pts',(-0.313685993055972,1.81141522451351,
8.00004705882353));
#18262=CARTESIAN_POINT('Ctrl Pts',(-1.41760501663887,0.93657834333742,8.08904988558308));
#18263=CARTESIAN_POINT('Ctrl Pts',(-1.55429061267928,0.209883225510418,
8.14101545744067));
#18264=CARTESIAN_POINT('Ctrl Pts',(-1.55334023889256,0.000780906153647377,
8.1559437743963));
#18265=CARTESIAN_POINT('Ctrl Pts',(-1.55374137824673,0.00106655561326607,
7.59405622560371));
#18266=CARTESIAN_POINT('Ctrl Pts',(-1.55164618369287,-0.331207576264562,
7.61779347869231));
#18267=CARTESIAN_POINT('Ctrl Pts',(-1.28426886371588,-1.18542758840111,
7.67859806542946));
#18268=CARTESIAN_POINT('Ctrl Pts',(0.122279206149944,-1.83480779990519,
7.77646998581516));
#18269=CARTESIAN_POINT('Ctrl Pts',(1.6083563717128,-0.891439258304551,7.88767198676082));
#18270=CARTESIAN_POINT('Ctrl Pts',(1.6207309884821,0.868737834600438,7.99887398770647));
#18271=CARTESIAN_POINT('Ctrl Pts',(0.148065176955119,1.83290543012718,8.11007598865213));
#18272=CARTESIAN_POINT('Ctrl Pts',(-1.27502705969297,1.20001188521837,8.20847006795121));
#18273=CARTESIAN_POINT('Ctrl Pts',(-1.55158956867716,0.33835081793624,8.26979681360173));
#18274=CARTESIAN_POINT('Ctrl Pts',(-1.55390047929932,-0.00114565379145014,
8.29405622560371));
#18275=CARTESIAN_POINT('Origin',(0.,0.,-1.2940562256037));
#18276=CARTESIAN_POINT('',(-1.55606381661923,-0.00136607279268914,6.7559437743963));
#18277=CARTESIAN_POINT('',(-1.55777357837665,0.000601989522525624,6.8940562256037));
#18278=CARTESIAN_POINT('',(-1.5555,-1.46451138874614E-13,-1.2940562256037));
#18279=CARTESIAN_POINT('Ctrl Pts',(-1.55606381661923,-0.00136607279268905,
6.7559437743963));
#18280=CARTESIAN_POINT('Ctrl Pts',(-1.5569964770826,-0.103043004100637,
6.76323506528381));
#18281=CARTESIAN_POINT('Ctrl Pts',(-1.50158858796583,-0.720192082985852,
6.80756361107328));
#18282=CARTESIAN_POINT('Ctrl Pts',(-0.676971321141057,-1.70919056845102,
6.8889294117647));
#18283=CARTESIAN_POINT('Ctrl Pts',(1.06848490487467,-1.49598214718639,7.00004117647059));
#18284=CARTESIAN_POINT('Ctrl Pts',(1.83636576494725,0.0859262661083765,
7.11115294117646));
#18285=CARTESIAN_POINT('Ctrl Pts',(0.924123786330422,1.58921924510457,7.22226470588235));
#18286=CARTESIAN_POINT('Ctrl Pts',(-0.833615098607335,1.63850800634715,
7.33337647058823));
#18287=CARTESIAN_POINT('Ctrl Pts',(-1.53117800274423,0.622142797307338,
7.41126949342621));
#18288=CARTESIAN_POINT('Ctrl Pts',(-1.55774976411747,0.0540350978509258,
7.45212526136224));
#18289=CARTESIAN_POINT('Ctrl Pts',(-1.55738256817027,0.000903178930570731,
7.4559437743963));
#18290=CARTESIAN_POINT('Ctrl Pts',(-1.55777357837665,0.000601989522525581,
6.8940562256037));
#18291=CARTESIAN_POINT('Ctrl Pts',(-1.55539426374015,-0.481439308478815,
6.92872281013432));
#18292=CARTESIAN_POINT('Ctrl Pts',(-1.05653937162455,-1.48315563828813,
7.0004567283135));
#18293=CARTESIAN_POINT('Ctrl Pts',(0.649252195647424,-1.72044892818251,
7.10925798014122));
#18294=CARTESIAN_POINT('Ctrl Pts',(1.79778702933405,-0.386567926277561,
7.22045998108688));
#18295=CARTESIAN_POINT('Ctrl Pts',(1.29904832373936,1.30151698160267,7.33166198203254));
#18296=CARTESIAN_POINT('Ctrl Pts',(-0.389980372076409,1.79704983321667,
7.44286398297819));
#18297=CARTESIAN_POINT('Ctrl Pts',(-1.43741330909764,0.891691889173598,
7.53032873083525));
#18298=CARTESIAN_POINT('Ctrl Pts',(-1.55491797235757,0.18766105875093,7.58072614504376));
#18299=CARTESIAN_POINT('Ctrl Pts',(-1.55374137824673,0.00106655561326607,
7.59405622560371));
#18300=CARTESIAN_POINT('Origin',(0.,0.,-1.2940562256037));
#18301=CARTESIAN_POINT('',(-1.55295095520957,-2.70144831846062E-5,6.0559437743963));
#18302=CARTESIAN_POINT('',(-1.55554339860443,-0.00142338748566243,6.19405622560371));
#18303=CARTESIAN_POINT('',(-1.5555,-1.46451138874614E-13,-1.2940562256037));
#18304=CARTESIAN_POINT('Ctrl Pts',(-1.55295123974832,-2.70114676757111E-5,
6.0559437743963));
#18305=CARTESIAN_POINT('Ctrl Pts',(-1.55299120405527,-0.257934102682435,
6.07434486920538));
#18306=CARTESIAN_POINT('Ctrl Pts',(-1.37002901128568,-1.03489667794099,
6.12978321891642));
#18307=CARTESIAN_POINT('Ctrl Pts',(-0.143167133221453,-1.83279178845155,
6.2222588235294));
#18308=CARTESIAN_POINT('Ctrl Pts',(1.46192436006299,-1.11462986392232,6.3333705882353));
#18309=CARTESIAN_POINT('Ctrl Pts',(1.72947592303562,0.623326238098233,6.44448235294117));
#18310=CARTESIAN_POINT('Ctrl Pts',(0.414699995127109,1.79099036343795,6.55559411764706));
#18311=CARTESIAN_POINT('Ctrl Pts',(-1.16831716986105,1.35095029518097,6.65941459146543));
#18312=CARTESIAN_POINT('Ctrl Pts',(-1.55225888207347,0.413440905347305,
6.72619781038185));
#18313=CARTESIAN_POINT('Ctrl Pts',(-1.55606381661923,-0.00136607279268905,
6.7559437743963));
#18314=CARTESIAN_POINT('Ctrl Pts',(-1.55554339860443,-0.00142338748566248,
6.19405622560371));
#18315=CARTESIAN_POINT('Ctrl Pts',(-1.55664045555565,-0.120456394769041,
6.2025848079278));
#18316=CARTESIAN_POINT('Ctrl Pts',(-1.48977304843445,-0.755616611367758,
6.24818072390044));
#18317=CARTESIAN_POINT('Ctrl Pts',(-0.618426992791356,-1.73176817298442,
6.33084397352162));
#18318=CARTESIAN_POINT('Ctrl Pts',(1.12039486833334,-1.45814549642773,6.4420459744673));
#18319=CARTESIAN_POINT('Ctrl Pts',(1.83262304280178,0.151544492417154,6.55324797541294));
#18320=CARTESIAN_POINT('Ctrl Pts',(0.865658194202354,1.62237752769619,6.6644499763586));
#18321=CARTESIAN_POINT('Ctrl Pts',(-0.894490612933678,1.60666097558597,
6.77565197730426));
#18322=CARTESIAN_POINT('Ctrl Pts',(-1.54182702766399,0.582629063158458,
6.85218739371929));
#18323=CARTESIAN_POINT('Ctrl Pts',(-1.55793835196459,0.0339845749906982,
6.89165547648577));
#18324=CARTESIAN_POINT('Ctrl Pts',(-1.55777357837665,0.000601989522525581,
6.8940562256037));
#18325=CARTESIAN_POINT('Origin',(0.,0.,-1.2940562256037));
#18326=CARTESIAN_POINT('',(-1.55596473934061,0.00138061827089577,5.3559437743963));
#18327=CARTESIAN_POINT('',(-1.55296794440831,0.000212393646609743,5.49405622560371));
#18328=CARTESIAN_POINT('',(-1.5555,-1.46451138874614E-13,-1.2940562256037));
#18329=CARTESIAN_POINT('Ctrl Pts',(-1.55596473934061,0.00138061827089576,
5.3559437743963));
#18330=CARTESIAN_POINT('Ctrl Pts',(-1.55217587900794,-0.41021582115075,
5.38545467312695));
#18331=CARTESIAN_POINT('Ctrl Pts',(-1.17326717115581,-1.34454702402952,
5.45200282675955));
#18332=CARTESIAN_POINT('Ctrl Pts',(0.403355110511087,-1.79357944420943,
5.55558823529412));
#18333=CARTESIAN_POINT('Ctrl Pts',(1.72549575760574,-0.634260954463495,
5.6667));
#18334=CARTESIAN_POINT('Ctrl Pts',(1.46895043569095,1.10535387335637,5.77781176470588));
#18335=CARTESIAN_POINT('Ctrl Pts',(-0.131563094636045,1.83366128824048,
5.88892352941177));
#18336=CARTESIAN_POINT('Ctrl Pts',(-1.36658225210923,1.04153952669523,5.98163419930856));
#18337=CARTESIAN_POINT('Ctrl Pts',(-1.55291076491625,0.261174720866106,
6.03730761430341));
#18338=CARTESIAN_POINT('Ctrl Pts',(-1.55295123974832,-2.70114676757111E-5,
6.0559437743963));
#18339=CARTESIAN_POINT('Ctrl Pts',(-1.55296794440831,0.000212393646609865,
5.49405622560371));
#18340=CARTESIAN_POINT('Ctrl Pts',(-1.55263586609147,-0.272499132194598,
5.51351413936982));
#18341=CARTESIAN_POINT('Ctrl Pts',(-1.35422347770915,-1.06517810244381,
5.57003938678448));
#18342=CARTESIAN_POINT('Ctrl Pts',(-0.089495975882287,-1.83669905549533,
5.66363196784771));
#18343=CARTESIAN_POINT('Ctrl Pts',(1.49519291292304,-1.07045369039924,5.77483396879335));
#18344=CARTESIAN_POINT('Ctrl Pts',(1.70986873918469,0.676625335695913,5.88603596973901));
#18345=CARTESIAN_POINT('Ctrl Pts',(0.357828666998206,1.80372713991337,5.99723797068467));
#18346=CARTESIAN_POINT('Ctrl Pts',(-1.19324218206278,1.31842435999021,6.09991138930622));
#18347=CARTESIAN_POINT('Ctrl Pts',(-1.55187237400387,0.396890571994748,
6.16551747427924));
#18348=CARTESIAN_POINT('Ctrl Pts',(-1.55554339860443,-0.00142338748566248,
6.19405622560371));
#18349=CARTESIAN_POINT('Origin',(0.,0.,-1.2940562256037));
#18350=CARTESIAN_POINT('',(-1.55745457732731,-0.00085669689206486,4.6559437743963));
#18351=CARTESIAN_POINT('',(-1.55632403677708,0.00132295834575361,4.7940562256037));
#18352=CARTESIAN_POINT('',(-1.5555,-1.46451138874614E-13,-1.2940562256037));
#18353=CARTESIAN_POINT('Ctrl Pts',(-1.55745457732731,-0.000856696892064714,
4.6559437743963));
#18354=CARTESIAN_POINT('Ctrl Pts',(-1.55778497931963,-0.0507117794212508,
4.65952722214655));
#18355=CARTESIAN_POINT('Ctrl Pts',(-1.53299973239953,-0.615518763747496,
4.70014792479876));
#18356=CARTESIAN_POINT('Ctrl Pts',(-0.843969773291502,-1.63319857630279,
4.77780588235294));
#18357=CARTESIAN_POINT('Ctrl Pts',(0.914045851976043,-1.59503691128215,
4.88891764705882));
#18358=CARTESIAN_POINT('Ctrl Pts',(1.83578508816481,-0.0975483364234787,
5.0000294117647));
#18359=CARTESIAN_POINT('Ctrl Pts',(1.07793273566426,1.48918890180207,5.11114117647059));
#18360=CARTESIAN_POINT('Ctrl Pts',(-0.666138955726334,1.7134414082573,5.22225294117646));
#18361=CARTESIAN_POINT('Ctrl Pts',(-1.49940020022205,0.726840308291178,
5.30385380715171));
#18362=CARTESIAN_POINT('Ctrl Pts',(-1.55693103699923,0.106352731462292,
5.34841741822499));
#18363=CARTESIAN_POINT('Ctrl Pts',(-1.55596473934061,0.00138061827089576,
5.3559437743963));
#18364=CARTESIAN_POINT('Ctrl Pts',(-1.55632403677708,0.0013229583457536,
4.7940562256037));
#18365=CARTESIAN_POINT('Ctrl Pts',(-1.55249345266231,-0.422243736756442,
4.82444347081184));
#18366=CARTESIAN_POINT('Ctrl Pts',(-1.15449033772237,-1.36882487339263,
4.89189804966852));
#18367=CARTESIAN_POINT('Ctrl Pts',(0.447130949584586,-1.78368911643119,
4.99641996217376));
#18368=CARTESIAN_POINT('Ctrl Pts',(1.74141681985029,-0.590711782254083,
5.10762196311942));
#18369=CARTESIAN_POINT('Ctrl Pts',(1.44007996484097,1.14352203521175,5.21882396406507));
#18370=CARTESIAN_POINT('Ctrl Pts',(-0.18077114541208,1.82997124106871,5.33002596501073));
#18371=CARTESIAN_POINT('Ctrl Pts',(-1.38135491130028,1.01294047027372,5.42177005219028));
#18372=CARTESIAN_POINT('Ctrl Pts',(-1.55326847542029,0.247016435592901,
5.47644680572127));
#18373=CARTESIAN_POINT('Ctrl Pts',(-1.55296794440831,0.000212393646609865,
5.49405622560371));
#18374=CARTESIAN_POINT('Origin',(0.,0.,-1.2940562256037));
#18375=CARTESIAN_POINT('',(-1.55339110712961,-0.000825623642478797,3.9559437743963));
#18376=CARTESIAN_POINT('',(-1.55725058804626,-0.000987513992002087,4.0940562256037));
#18377=CARTESIAN_POINT('',(-1.5555,-1.46451138874614E-13,-1.2940562256037));
#18378=CARTESIAN_POINT('Ctrl Pts',(-1.55339110712961,-0.000825623642478918,
3.9559437743963));
#18379=CARTESIAN_POINT('Ctrl Pts',(-1.55438254706171,-0.206618413857449,
3.97063702606812));
#18380=CARTESIAN_POINT('Ctrl Pts',(-1.42060545887363,-0.929915671591215,
4.0223675326419));
#18381=CARTESIAN_POINT('Ctrl Pts',(-0.325144523748834,-1.80939315974833,
4.11113529411765));
#18382=CARTESIAN_POINT('Ctrl Pts',(1.34353857429153,-1.25480144535206,4.22224705882353));
#18383=CARTESIAN_POINT('Ctrl Pts',(1.7829949491126,0.447829855308947,4.33335882352941));
#18384=CARTESIAN_POINT('Ctrl Pts',(0.591158348240881,1.74073386109778,4.44447058823529));
#18385=CARTESIAN_POINT('Ctrl Pts',(-1.08565831565865,1.45067662979582,4.55199890519093));
#18386=CARTESIAN_POINT('Ctrl Pts',(-1.55437006059814,0.464572809188085,
4.62248996724459));
#18387=CARTESIAN_POINT('Ctrl Pts',(-1.55745457732731,-0.000856696892064714,
4.6559437743963));
#18388=CARTESIAN_POINT('Ctrl Pts',(-1.55725058804626,-0.000987513992001905,
4.0940562256037));
#18389=CARTESIAN_POINT('Ctrl Pts',(-1.55768831435815,-0.060125904161909,
4.09830546860531));
#18390=CARTESIAN_POINT('Ctrl Pts',(-1.52777409038815,-0.634697902152519,
4.13962204525546));
#18391=CARTESIAN_POINT('Ctrl Pts',(-0.813442378520323,-1.64917689984389,
4.21800595555418));
#18392=CARTESIAN_POINT('Ctrl Pts',(0.945308337362415,-1.57729676898942,
4.32920795649982));
#18393=CARTESIAN_POINT('Ctrl Pts',(1.83789338383513,-0.0601735806349488,
4.44040995744549));
#18394=CARTESIAN_POINT('Ctrl Pts',(1.04645630737228,1.51208536363268,4.55161195839114));
#18395=CARTESIAN_POINT('Ctrl Pts',(-0.703826144888774,1.69885305660096,
4.66281395933679));
#18396=CARTESIAN_POINT('Ctrl Pts',(-1.5071493991015,0.703327095585107,4.74362871507432));
#18397=CARTESIAN_POINT('Ctrl Pts',(-1.5571661216877,0.0944364658163476,
4.78737613716329));
#18398=CARTESIAN_POINT('Ctrl Pts',(-1.55632403677708,0.0013229583457536,
4.7940562256037));
#18399=CARTESIAN_POINT('Origin',(0.,0.,-1.2940562256037));
#18400=CARTESIAN_POINT('',(-1.55444728254952,0.00131753317857479,3.2559437743963));
#18401=CARTESIAN_POINT('',(-1.55328288481294,-0.000737459407344904,3.3940562256037));
#18402=CARTESIAN_POINT('',(-1.5555,-1.46451138874614E-13,-1.2940562256037));
#18403=CARTESIAN_POINT('Ctrl Pts',(-1.55444728254952,0.00131753317857487,
3.2559437743963));
#18404=CARTESIAN_POINT('Ctrl Pts',(-1.55154249309476,-0.359460968451768,
3.28174682998969));
#18405=CARTESIAN_POINT('Ctrl Pts',(-1.24689466125852,-1.24251939835746,
3.34458714048504));
#18406=CARTESIAN_POINT('Ctrl Pts',(0.2225644970039,-1.82485276462931,3.44446470588235));
#18407=CARTESIAN_POINT('Ctrl Pts',(1.65367987605646,-0.803097400934551,
3.55557647058823));
#18408=CARTESIAN_POINT('Ctrl Pts',(1.57181488059719,0.953425691385454,3.66668823529412));
#18409=CARTESIAN_POINT('Ctrl Pts',(0.05186921357973,1.83764309716413,3.7778));
#18410=CARTESIAN_POINT('Ctrl Pts',(-1.30826166492629,1.14597286376508,3.87421851303406));
#18411=CARTESIAN_POINT('Ctrl Pts',(-1.55188342608391,0.312123128070615,
3.93359977116616));
#18412=CARTESIAN_POINT('Ctrl Pts',(-1.55339110712961,-0.000825623642478918,
3.9559437743963));
#18413=CARTESIAN_POINT('Ctrl Pts',(-1.55328288481294,-0.000737459407344626,
3.3940562256037));
#18414=CARTESIAN_POINT('Ctrl Pts',(-1.55419278937645,-0.213364380143022,
3.40923480004733));
#18415=CARTESIAN_POINT('Ctrl Pts',(-1.41432753571211,-0.944097869976176,
3.4614807081395));
#18416=CARTESIAN_POINT('Ctrl Pts',(-0.300084107876245,-1.81422779119842,
3.55079394988024));
#18417=CARTESIAN_POINT('Ctrl Pts',(1.36219708122283,-1.23527003608861,3.66199595082589));
#18418=CARTESIAN_POINT('Ctrl Pts',(1.77632642388981,0.475539047756765,3.77319795177155));
#18419=CARTESIAN_POINT('Ctrl Pts',(0.562846122986205,1.75062194433623,3.8843999527172));
#18420=CARTESIAN_POINT('Ctrl Pts',(-1.10028173365827,1.43421840050251,3.99135271066126));
#18421=CARTESIAN_POINT('Ctrl Pts',(-1.55386990546895,0.455754792479586,
4.06123813495675));
#18422=CARTESIAN_POINT('Ctrl Pts',(-1.55725058804626,-0.000987513992001905,
4.0940562256037));
#18423=CARTESIAN_POINT('Origin',(0.,0.,-1.2940562256037));
#18424=CARTESIAN_POINT('',(-1.5580472770765,3.22739011431662E-5,2.5559437743963));
#18425=CARTESIAN_POINT('',(-1.55455103081039,0.00134678255213586,2.6940562256037));
#18426=CARTESIAN_POINT('',(-1.5555,-1.46451138874614E-13,-1.2940562256037));
#18427=CARTESIAN_POINT('Ctrl Pts',(-1.5580472770765,3.22739011430483E-5,
2.5559437743963));
#18428=CARTESIAN_POINT('Ctrl Pts',(-1.55789051448101,-0.513002401697162,
2.59285663391126));
#18429=CARTESIAN_POINT('Ctrl Pts',(-1.00059908603036,-1.54109252504942,
2.66680674832818));
#18430=CARTESIAN_POINT('Ctrl Pts',(0.750502303520728,-1.67820405842339,
2.77779411764705));
#18431=CARTESIAN_POINT('Ctrl Pts',(1.81691877690325,-0.280051291770722,
2.88890588235294));
#18432=CARTESIAN_POINT('Ctrl Pts',(1.221004776546,1.37432525375672,3.00001764705882));
#18433=CARTESIAN_POINT('Ctrl Pts',(-0.492027652059084,1.77130780998173,
3.11112941176471));
#18434=CARTESIAN_POINT('Ctrl Pts',(-1.4616245475244,0.831846153950699,3.1964381208772));
#18435=CARTESIAN_POINT('Ctrl Pts',(-1.55571197709572,0.158394185549965,
3.24470957508773));
#18436=CARTESIAN_POINT('Ctrl Pts',(-1.55444728254952,0.00131753317857487,
3.2559437743963));
#18437=CARTESIAN_POINT('Ctrl Pts',(-1.55455103081039,0.00134678255213593,
2.6940562256037));
#18438=CARTESIAN_POINT('Ctrl Pts',(-1.55153631123715,-0.363632076962094,
2.72016413148935));
#18439=CARTESIAN_POINT('Ctrl Pts',(-1.2410339082364,-1.25141700119195,2.78333937102354));
#18440=CARTESIAN_POINT('Ctrl Pts',(0.239078896742882,-1.82327020255007,
2.88358194420631));
#18441=CARTESIAN_POINT('Ctrl Pts',(1.66194822130476,-0.787020368122459,
2.99478394515195));
#18442=CARTESIAN_POINT('Ctrl Pts',(1.56201018579718,0.970359278599158,3.10598594609762));
#18443=CARTESIAN_POINT('Ctrl Pts',(0.0308358597469676,1.83861961806662,
3.21718794704326));
#18444=CARTESIAN_POINT('Ctrl Pts',(-1.31573769524687,1.1336310555357,3.3132113735453));
#18445=CARTESIAN_POINT('Ctrl Pts',(-1.55197072720788,0.305888138784002,
3.37216746639878));
#18446=CARTESIAN_POINT('Ctrl Pts',(-1.55328288481294,-0.000737459407344626,
3.3940562256037));
#18447=CARTESIAN_POINT('Origin',(0.,0.,-1.2940562256037));
#18448=CARTESIAN_POINT('',(-1.55454106205097,-0.00133830406313126,1.8559437743963));
#18449=CARTESIAN_POINT('',(-1.55805738347505,7.8333006204296E-6,1.9940562256037));
#18450=CARTESIAN_POINT('',(-1.5555,-1.46451138874614E-13,-1.2940562256037));
#18451=CARTESIAN_POINT('Ctrl Pts',(-1.55454106205097,-0.00133830406313111,
1.8559437743963));
#18452=CARTESIAN_POINT('Ctrl Pts',(-1.55580278448011,-0.154912931015377,
1.86692918293086));
#18453=CARTESIAN_POINT('Ctrl Pts',(-1.4643553294945,-0.824794260236109,
1.91495184636739));
#18454=CARTESIAN_POINT('Ctrl Pts',(-0.503883253349445,-1.76797174153445,
2.00001176470588));
#18455=CARTESIAN_POINT('Ctrl Pts',(1.21177025569706,-1.38247440008765,2.11112352941176));
#18456=CARTESIAN_POINT('Ctrl Pts',(1.81875417317235,0.267872803846544,2.22223529411764));
#18457=CARTESIAN_POINT('Ctrl Pts',(0.761728374059259,1.67313849696631,2.33334705882353));
#18458=CARTESIAN_POINT('Ctrl Pts',(-0.992215910389441,1.54762080750275,
2.44445882352941));
#18459=CARTESIAN_POINT('Ctrl Pts',(-1.5572623887173,0.518253196217567,2.51865772872033));
#18460=CARTESIAN_POINT('Ctrl Pts',(-1.55804780536241,0.00176118756036677,
2.5558193790093));
#18461=CARTESIAN_POINT('Ctrl Pts',(-1.5580472770765,3.22739011430483E-5,
2.5559437743963));
#18462=CARTESIAN_POINT('Ctrl Pts',(-1.55805738347505,7.83330062046083E-6,
1.9940562256037));
#18463=CARTESIAN_POINT('Ctrl Pts',(-1.55801899566519,-0.514746844163175,
2.03109346293137));
#18464=CARTESIAN_POINT('Ctrl Pts',(-0.997193073467916,-1.54474611801162,
2.1051980339076));
#18465=CARTESIAN_POINT('Ctrl Pts',(0.757683106401647,-1.67552656471375,
2.21636993853236));
#18466=CARTESIAN_POINT('Ctrl Pts',(1.81878565659978,-0.271093501731151,
2.32757193947802));
#18467=CARTESIAN_POINT('Ctrl Pts',(1.2133740808,1.38173669240563,2.43877394042368));
#18468=CARTESIAN_POINT('Ctrl Pts',(-0.50382603046139,1.76851131819754,2.54997594136933));
#18469=CARTESIAN_POINT('Ctrl Pts',(-1.46460308673025,0.824478033792379,
2.63507003642934));
#18470=CARTESIAN_POINT('Ctrl Pts',(-1.55581653259107,0.154555525656757,
2.6830967978408));
#18471=CARTESIAN_POINT('Ctrl Pts',(-1.55455103081039,0.00134678255213593,
2.6940562256037));
#18472=CARTESIAN_POINT('Origin',(0.,0.,-1.2940562256037));
#18473=CARTESIAN_POINT('',(-1.55333654104773,0.00077999677327307,1.1559437743963));
#18474=CARTESIAN_POINT('',(-1.55457410202289,-0.00135137241159503,1.2940562256037));
#18475=CARTESIAN_POINT('',(-1.5555,-1.46451138874614E-13,-1.2940562256037));
#18476=CARTESIAN_POINT('Ctrl Pts',(-1.55333654104773,0.000779996773273093,
1.1559437743963));
#18477=CARTESIAN_POINT('Ctrl Pts',(-1.55193441184992,-0.308712050983944,
1.17803898685243));
#18478=CARTESIAN_POINT('Ctrl Pts',(-1.31241259724573,-1.13899385066835,
1.23717145421053));
#18479=CARTESIAN_POINT('Ctrl Pts',(0.0395573460867233,-1.83794734661457,
1.33334117647059));
#18480=CARTESIAN_POINT('Ctrl Pts',(1.56539206925502,-0.963935520329204,
1.44445294117647));
#18481=CARTESIAN_POINT('Ctrl Pts',(1.65902311109036,0.792001314055404,1.55556470588235));
#18482=CARTESIAN_POINT('Ctrl Pts',(0.234784819358076,1.82332048051019,1.66667647058823));
#18483=CARTESIAN_POINT('Ctrl Pts',(-1.24221255679906,1.24941902193381,1.76680282675955));
#18484=CARTESIAN_POINT('Ctrl Pts',(-1.55154889304983,0.362863225147233,
1.8298919280289));
#18485=CARTESIAN_POINT('Ctrl Pts',(-1.55454106205097,-0.00133830406313111,
1.8559437743963));
#18486=CARTESIAN_POINT('Ctrl Pts',(-1.55457410202289,-0.00135137241159506,
1.2940562256037));
#18487=CARTESIAN_POINT('Ctrl Pts',(-1.55583838883925,-0.153712992066033,
1.30495546072484));
#18488=CARTESIAN_POINT('Ctrl Pts',(-1.46525911062305,-0.822772247294108,
1.35292202949453));
#18489=CARTESIAN_POINT('Ctrl Pts',(-0.506691785521986,-1.76769208329225,
1.43795593191277));
#18490=CARTESIAN_POINT('Ctrl Pts',(1.21113283005724,-1.38370173748454,1.54915793285843));
#18491=CARTESIAN_POINT('Ctrl Pts',(1.81922269924897,0.268145221691032,1.66035993380409));
#18492=CARTESIAN_POINT('Ctrl Pts',(0.760397896971566,1.67429621989364,1.77156193474974));
#18493=CARTESIAN_POINT('Ctrl Pts',(-0.99516307107971,1.54632579451077,1.8827639356954));
#18494=CARTESIAN_POINT('Ctrl Pts',(-1.55786775595712,0.516017344817124,
1.95692869931338));
#18495=CARTESIAN_POINT('Ctrl Pts',(-1.55805741466885,0.000426121031216267,
1.99402612928282));
#18496=CARTESIAN_POINT('Ctrl Pts',(-1.55805738347505,7.83330062046083E-6,
1.9940562256037));
#18497=CARTESIAN_POINT('Origin',(0.,0.,-1.2940562256037));
#18498=CARTESIAN_POINT('',(-1.55735939632673,0.00101326450419681,0.455943774396298));
#18499=CARTESIAN_POINT('',(-1.55326674879324,0.000737490386717859,0.594056225603704));
#18500=CARTESIAN_POINT('',(-1.5555,-1.46451138874614E-13,-1.2940562256037));
#18501=CARTESIAN_POINT('Ctrl Pts',(-1.55735939632673,0.00101326450419686,
0.455943774396298));
#18502=CARTESIAN_POINT('Ctrl Pts',(-1.55415403990615,-0.460986485095401,
0.489148790774002));
#18503=CARTESIAN_POINT('Ctrl Pts',(-1.09150770385912,-1.44424025370235,
0.559391062053666));
#18504=CARTESIAN_POINT('Ctrl Pts',(0.579500018064921,-1.74455968620895,
0.666670588235291));
#18505=CARTESIAN_POINT('Ctrl Pts',(1.77994595636936,-0.459814902815864,
0.777782352941175));
#18506=CARTESIAN_POINT('Ctrl Pts',(1.35191942796293,1.24579875779621,0.888894117647056));
#18507=CARTESIAN_POINT('Ctrl Pts',(-0.31301785631821,1.81151698861828,1.00000588235294));
#18508=CARTESIAN_POINT('Ctrl Pts',(-1.41742989907648,0.936970735614399,
1.08902243460269));
#18509=CARTESIAN_POINT('Ctrl Pts',(-1.55428474075524,0.210076165498259,
1.14100173195047));
#18510=CARTESIAN_POINT('Ctrl Pts',(-1.55333654104773,0.000779996773273093,
1.1559437743963));
#18511=CARTESIAN_POINT('Ctrl Pts',(-1.55326674879324,0.000737490386717929,
0.594056225603704));
#18512=CARTESIAN_POINT('Ctrl Pts',(-1.55198188529325,-0.305056076963429,
0.615884792166863));
#18513=CARTESIAN_POINT('Ctrl Pts',(-1.31673706663562,-1.13196023879971,
0.674780692378575));
#18514=CARTESIAN_POINT('Ctrl Pts',(0.0278603330084876,-1.83865390028585,
0.770743926238836));
#18515=CARTESIAN_POINT('Ctrl Pts',(1.5604328654528,-0.972896783194139,0.881945927184494));
#18516=CARTESIAN_POINT('Ctrl Pts',(1.66322297628929,0.784329206349798,0.993147928130148));
#18517=CARTESIAN_POINT('Ctrl Pts',(0.242033178606095,1.82287837028977,1.10434992907581));
#18518=CARTESIAN_POINT('Ctrl Pts',(-1.23989296747105,1.25308568603502,1.20465269490032));
#18519=CARTESIAN_POINT('Ctrl Pts',(-1.55153866131449,0.364455386558259,
1.26788812707629));
#18520=CARTESIAN_POINT('Ctrl Pts',(-1.55457410202289,-0.00135137241159506,
1.2940562256037));
#18521=CARTESIAN_POINT('Origin',(0.,0.,9.5));
#18522=CARTESIAN_POINT('',(-1.8436644593731,-0.000635433610831735,9.15893008989225));
#18523=CARTESIAN_POINT('Ctrl Pts',(0.964986447796868,1.2199923793075,9.4445));
#18524=CARTESIAN_POINT('Ctrl Pts',(1.01353513125755,1.18505085067097,9.44178677406621));
#18525=CARTESIAN_POINT('Ctrl Pts',(1.0597539884705,1.14720650264821,9.43908619037108));
#18526=CARTESIAN_POINT('Ctrl Pts',(1.10357643916964,1.10678728284429,9.43639370111374));
#18527=CARTESIAN_POINT('Ctrl Pts',(1.14671113352339,1.0670024085517,9.43374346820086));
#18528=CARTESIAN_POINT('Ctrl Pts',(1.18752436163327,1.02472203468752,9.43110107764874));
#18529=CARTESIAN_POINT('Ctrl Pts',(1.22592701109647,0.980220056324443,9.4284621924353));
#18530=CARTESIAN_POINT('Ctrl Pts',(1.24656064684413,0.956309268281708,9.42704432681834));
#18531=CARTESIAN_POINT('Ctrl Pts',(1.2664979086022,0.931756532766836,9.42562747315155));
#18532=CARTESIAN_POINT('Ctrl Pts',(1.28572135928109,0.906600809401326,9.42421095871337));
#18533=CARTESIAN_POINT('Ctrl Pts',(1.29315226707552,0.896876756006653,9.42366339894611));
#18534=CARTESIAN_POINT('Ctrl Pts',(1.30047431632806,0.887065294343418,9.42311604538434));
#18535=CARTESIAN_POINT('Ctrl Pts',(1.30768090461229,0.877176902486747,9.4225693022564));
#18536=CARTESIAN_POINT('Ctrl Pts',(1.34465595997822,0.826442238321084,9.4197641111411));
#18537=CARTESIAN_POINT('Ctrl Pts',(1.37864083403329,0.773625333680106,9.41697158537819));
#18538=CARTESIAN_POINT('Ctrl Pts',(1.40953528457578,0.719059333620718,9.41418667925324));
#18539=CARTESIAN_POINT('Ctrl Pts',(1.44068034022624,0.664050713022807,9.41137918293207));
#18540=CARTESIAN_POINT('Ctrl Pts',(1.46868519868955,0.607263591678243,9.40857943036595));
#18541=CARTESIAN_POINT('Ctrl Pts',(1.4934057683288,0.549006709906255,9.40578225205449));
#18542=CARTESIAN_POINT('Ctrl Pts',(1.49984356600261,0.533835295030795,9.40505380330555));
#18543=CARTESIAN_POINT('Ctrl Pts',(1.50605838114916,0.518564071644944,9.40432552914253));
#18544=CARTESIAN_POINT('Ctrl Pts',(1.51204713790707,0.503198254185902,9.40359733826241));
#18545=CARTESIAN_POINT('Ctrl Pts',(1.51578438435043,0.493609311276813,9.40314291526832));
#18546=CARTESIAN_POINT('Ctrl Pts',(1.51943283421544,0.483985318888239,9.40268861051374));
#18547=CARTESIAN_POINT('Ctrl Pts',(1.52298881285553,0.474336147548569,9.40223480218929));
#18548=CARTESIAN_POINT('Ctrl Pts',(1.54512657800669,0.414265176757972,9.39940961589683));
#18549=CARTESIAN_POINT('Ctrl Pts',(1.56372018959743,0.353128682437969,9.39659929425661));
#18550=CARTESIAN_POINT('Ctrl Pts',(1.57865714116174,0.291257786036896,9.39379872614803));
#18551=CARTESIAN_POINT('Ctrl Pts',(1.59350224792573,0.229767323360879,9.39101537826123));
#18552=CARTESIAN_POINT('Ctrl Pts',(1.60473597791275,0.167550465196752,9.38824166432918));
#18553=CARTESIAN_POINT('Ctrl Pts',(1.612201835455,0.104910300904696,9.38547256693499));
#18554=CARTESIAN_POINT('Ctrl Pts',(1.61736371100559,0.0616010453082987,
9.38355801980422));
#18555=CARTESIAN_POINT('Ctrl Pts',(1.62072348102385,0.0180889750237585,
9.38164567951963));
#18556=CARTESIAN_POINT('Ctrl Pts',(1.62221464959515,-0.0255281734684064,
9.379733887779));
#18557=CARTESIAN_POINT('Ctrl Pts',(1.62311301667558,-0.0518056923901331,
9.37858211272319));
#18558=CARTESIAN_POINT('Ctrl Pts',(1.6233329220732,-0.0781213723415495,
9.37743053676479));
#18559=CARTESIAN_POINT('Ctrl Pts',(1.6228574829942,-0.104453779990354,9.37627879728949));
#18560=CARTESIAN_POINT('Ctrl Pts',(1.62265929679902,-0.115430411724188,
9.3757986961061));
#18561=CARTESIAN_POINT('Ctrl Pts',(1.6223401558167,-0.126409918390069,9.37531856781002));
#18562=CARTESIAN_POINT('Ctrl Pts',(1.62189965557521,-0.137376114393304,
9.37483902548745));
#18563=CARTESIAN_POINT('Ctrl Pts',(1.6216428503266,-0.143769247530682,9.37455945927212));
#18564=CARTESIAN_POINT('Ctrl Pts',(1.62134478429418,-0.15015909919995,9.37428003787639));
#18565=CARTESIAN_POINT('Ctrl Pts',(1.62100533439947,-0.156545355045619,
9.37400075635211));
#18566=CARTESIAN_POINT('Ctrl Pts',(1.61776588850122,-0.217490816000868,
9.37133551060487));
#18567=CARTESIAN_POINT('Ctrl Pts',(1.61076184583078,-0.27810811078512,9.36868300338423));
#18568=CARTESIAN_POINT('Ctrl Pts',(1.60024388638002,-0.33815222699736,9.36603893410604));
#18569=CARTESIAN_POINT('Ctrl Pts',(1.58926239194622,-0.400842535992609,
9.36327833855545));
#18570=CARTESIAN_POINT('Ctrl Pts',(1.5744503497123,-0.462908874929355,9.3605269410697));
#18571=CARTESIAN_POINT('Ctrl Pts',(1.55603619221491,-0.524074243638481,
9.35777984704762));
#18572=CARTESIAN_POINT('Ctrl Pts',(1.54065020182884,-0.575181103947007,
9.35548450650763));
#18573=CARTESIAN_POINT('Ctrl Pts',(1.52274824032724,-0.625659260102185,
9.35319217042017));
#18574=CARTESIAN_POINT('Ctrl Pts',(1.50243626590723,-0.675341229990148,
9.35089998357483));
#18575=CARTESIAN_POINT('Ctrl Pts',(1.49675934867098,-0.689226656653057,
9.35025934890575));
#18576=CARTESIAN_POINT('Ctrl Pts',(1.49089404119114,-0.70304983797203,9.34961872589435));
#18577=CARTESIAN_POINT('Ctrl Pts',(1.48484234501078,-0.716806975404219,
9.34897805220743));
#18578=CARTESIAN_POINT('Ctrl Pts',(1.47962711111297,-0.728662608492026,
9.34842593210261));
#18579=CARTESIAN_POINT('Ctrl Pts',(1.47427261241135,-0.74047069735123,9.34787370156138));
#18580=CARTESIAN_POINT('Ctrl Pts',(1.46878946750842,-0.752209477846282,
9.34732223297784));
#18581=CARTESIAN_POINT('Ctrl Pts',(1.44124114383179,-0.811187259825758,
9.34455155386835));
#18582=CARTESIAN_POINT('Ctrl Pts',(1.41040240116235,-0.868527008616387,
9.34179496514958));
#18583=CARTESIAN_POINT('Ctrl Pts',(1.3765156583388,-0.923951665257498,9.33904765215105));
#18584=CARTESIAN_POINT('Ctrl Pts',(1.34221268254424,-0.98005710640542,9.33626659373598));
#18585=CARTESIAN_POINT('Ctrl Pts',(1.30478591472408,-1.03420112061383,9.3334950403091));
#18586=CARTESIAN_POINT('Ctrl Pts',(1.26443637894511,-1.08608026731007,9.33072799759508));
#18587=CARTESIAN_POINT('Ctrl Pts',(1.23112993903158,-1.1289038004399,9.32844394797434));
#18588=CARTESIAN_POINT('Ctrl Pts',(1.19583096929852,-1.17018410899034,9.32616297179209));
#18589=CARTESIAN_POINT('Ctrl Pts',(1.15863053726262,-1.20973500520381,9.32388226011456));
#18590=CARTESIAN_POINT('Ctrl Pts',(1.14503499841471,-1.22418956168373,9.32304873473553));
#18591=CARTESIAN_POINT('Ctrl Pts',(1.13118531407677,-1.23841295906892,9.32221524468542));
#18592=CARTESIAN_POINT('Ctrl Pts',(1.11708535825451,-1.25239547008276,9.32138165284865));
#18593=CARTESIAN_POINT('Ctrl Pts',(1.10886443632285,-1.26054791629624,9.32089563051642));
#18594=CARTESIAN_POINT('Ctrl Pts',(1.10055776106962,-1.26861897429176,9.3204095386295));
#18595=CARTESIAN_POINT('Ctrl Pts',(1.09217814991772,-1.27659553689908,9.31992403906899));
#18596=CARTESIAN_POINT('Ctrl Pts',(1.0442665456713,-1.32220265445632,9.31714812711039));
#18597=CARTESIAN_POINT('Ctrl Pts',(0.993885467018336,-1.36481211874555,
9.31438629338051));
#18598=CARTESIAN_POINT('Ctrl Pts',(0.941242813634035,-1.40412918747402,
9.31163369987499));
#18599=CARTESIAN_POINT('Ctrl Pts',(0.889258180215484,-1.4429548027032,9.30891551309799));
#18600=CARTESIAN_POINT('Ctrl Pts',(0.835067536107577,-1.47857067848576,
9.30620633698811));
#18601=CARTESIAN_POINT('Ctrl Pts',(0.778833889995821,-1.51065975001959,
9.30350151270422));
#18602=CARTESIAN_POINT('Ctrl Pts',(0.722586441970542,-1.54275669745372,
9.30079602455175));
#18603=CARTESIAN_POINT('Ctrl Pts',(0.664294246016674,-1.57132562044258,
9.29809489036176));
#18604=CARTESIAN_POINT('Ctrl Pts',(0.60428947258743,-1.59639249571732,9.2953934478619));
#18605=CARTESIAN_POINT('Ctrl Pts',(0.591343331742152,-1.60180072041865,
9.29481060664627));
#18606=CARTESIAN_POINT('Ctrl Pts',(0.57831739582737,-1.60704575229747,9.29422775107918));
#18607=CARTESIAN_POINT('Ctrl Pts',(0.565214891376733,-1.61212755946014,
9.2936448343374));
#18608=CARTESIAN_POINT('Ctrl Pts',(0.555972206658096,-1.6157123353007,9.29323363694519));
#18609=CARTESIAN_POINT('Ctrl Pts',(0.546693262642617,-1.61921511430512,
9.29282249204174));
#18610=CARTESIAN_POINT('Ctrl Pts',(0.537387803700891,-1.62263297583653,
9.29241175882646));
#18611=CARTESIAN_POINT('Ctrl Pts',(0.475984234705077,-1.64518628542356,
9.28970146957778));
#18612=CARTESIAN_POINT('Ctrl Pts',(0.413324985792773,-1.66408644383074,
9.2870044827103));
#18613=CARTESIAN_POINT('Ctrl Pts',(0.349771964499173,-1.67941338858561,
9.28431629702065));
#18614=CARTESIAN_POINT('Ctrl Pts',(0.284907818691178,-1.69505653440519,
9.2815726529738));
#18615=CARTESIAN_POINT('Ctrl Pts',(0.219111690562125,-1.70697771722454,
9.2788381769944));
#18616=CARTESIAN_POINT('Ctrl Pts',(0.152743105316565,-1.71521251897908,
9.27610808350735));
#18617=CARTESIAN_POINT('Ctrl Pts',(0.108619750041913,-1.72068720375785,
9.27429305483955));
#18618=CARTESIAN_POINT('Ctrl Pts',(0.0642428719693675,-1.72453152305287,
9.27247996318729));
#18619=CARTESIAN_POINT('Ctrl Pts',(0.0197153791249731,-1.72674355800955,
9.27066740233454));
#18620=CARTESIAN_POINT('Ctrl Pts',(-0.00935520099652008,-1.72818772509222,
9.26948403915532));
#18621=CARTESIAN_POINT('Ctrl Pts',(-0.0384900123738061,-1.72893595074551,
9.26830090222237));
#18622=CARTESIAN_POINT('Ctrl Pts',(-0.0676604159497131,-1.72898539458108,
9.26711760021896));
#18623=CARTESIAN_POINT('Ctrl Pts',(-0.0792958143034031,-1.72900511658189,
9.26664560845695));
#18624=CARTESIAN_POINT('Ctrl Pts',(-0.0909391905971971,-1.72891359625761,
9.26617349650779));
#18625=CARTESIAN_POINT('Ctrl Pts',(-0.102581232900295,-1.72871071219562,
9.26570154289531));
#18626=CARTESIAN_POINT('Ctrl Pts',(-0.170900558303332,-1.72752012192893,
9.26293196419191));
#18627=CARTESIAN_POINT('Ctrl Pts',(-0.238956647295054,-1.72250403767711,
9.26017659214973));
#18628=CARTESIAN_POINT('Ctrl Pts',(-0.30637923630299,-1.71371181735864,
9.25743063944084));
#18629=CARTESIAN_POINT('Ctrl Pts',(-0.373589954383447,-1.70494722599808,
9.25469331570268));
#18630=CARTESIAN_POINT('Ctrl Pts',(-0.440172255573728,-1.69243020084097,
9.25196535219159));
#18631=CARTESIAN_POINT('Ctrl Pts',(-0.505764774523597,-1.67615838081314,
9.24924200656954));
#18632=CARTESIAN_POINT('Ctrl Pts',(-0.571106403622123,-1.65994880011646,
9.24652907768082));
#18633=CARTESIAN_POINT('Ctrl Pts',(-0.635466898101783,-1.64001312037568,
9.24382073142206));
#18634=CARTESIAN_POINT('Ctrl Pts',(-0.698478020047089,-1.6162978205588,
9.24111227966534));
#18635=CARTESIAN_POINT('Ctrl Pts',(-0.714257342673809,-1.61035900602182,
9.24043402584651));
#18636=CARTESIAN_POINT('Ctrl Pts',(-0.729951945569458,-1.60418291559246,
9.23975576541181));
#18637=CARTESIAN_POINT('Ctrl Pts',(-0.745555812125029,-1.59776819932882,
9.23907742473836));
#18638=CARTESIAN_POINT('Ctrl Pts',(-0.758165841483652,-1.59258424315208,
9.23852923395649));
#18639=CARTESIAN_POINT('Ctrl Pts',(-0.7707186000527,-1.58724342153027,9.23798090121265));
#18640=CARTESIAN_POINT('Ctrl Pts',(-0.783190247921723,-1.58175442379625,
9.23743329902252));
#18641=CARTESIAN_POINT('Ctrl Pts',(-0.816912656931304,-1.56691258183734,
9.23595262339534));
#18642=CARTESIAN_POINT('Ctrl Pts',(-0.850075178494816,-1.55097461965651,
9.23447585783886));
#18643=CARTESIAN_POINT('Ctrl Pts',(-0.882621385021603,-1.53394288417305,
9.23300226905634));
#18644=CARTESIAN_POINT('Ctrl Pts',(-0.940729021590098,-1.50353461232764,
9.23037133996924));
#18645=CARTESIAN_POINT('Ctrl Pts',(-0.996873413800297,-1.46964284065132,
9.22775053721005));
#18646=CARTESIAN_POINT('Ctrl Pts',(-1.05092798108356,-1.43259472728442,
9.22513568749178));
#18647=CARTESIAN_POINT('Ctrl Pts',(-1.10572540080839,-1.39503747504446,
9.22248490283599));
#18648=CARTESIAN_POINT('Ctrl Pts',(-1.15837574574728,-1.35423590514407,
9.21984023596641));
#18649=CARTESIAN_POINT('Ctrl Pts',(-1.20872367105371,-1.3104847487346,9.21719733916479));
#18650=CARTESIAN_POINT('Ctrl Pts',(-1.23098837194441,-1.29113725020014,
9.21602860566852));
#18651=CARTESIAN_POINT('Ctrl Pts',(-1.25280246308233,-1.27121240133872,
9.21486021831921));
#18652=CARTESIAN_POINT('Ctrl Pts',(-1.27415061053865,-1.25073337083793,
9.21369180113468));
#18653=CARTESIAN_POINT('Ctrl Pts',(-1.28784402235457,-1.23759743954403,
9.21294233949107));
#18654=CARTESIAN_POINT('Ctrl Pts',(-1.301345702892,-1.224233470889,9.21219286557216));
#18655=CARTESIAN_POINT('Ctrl Pts',(-1.31465131341234,-1.2106473229253,9.21144328015282));
#18656=CARTESIAN_POINT('Ctrl Pts',(-1.32306845489082,-1.20205271320159,
9.21096909172567));
#18657=CARTESIAN_POINT('Ctrl Pts',(-1.33140768074567,-1.19336846646048,
9.21049482332023));
#18658=CARTESIAN_POINT('Ctrl Pts',(-1.33965658703659,-1.1846083807011,9.21002110694334));
#18659=CARTESIAN_POINT('Ctrl Pts',(-1.38683756934781,-1.13450362296938,
9.20731160786425));
#18660=CARTESIAN_POINT('Ctrl Pts',(-1.43115584257498,-1.08183136746067,
9.20461514627079));
#18661=CARTESIAN_POINT('Ctrl Pts',(-1.47246637362013,-1.0269335551328,9.20192723192248));
#18662=CARTESIAN_POINT('Ctrl Pts',(-1.51435673419381,-0.971265203868867,
9.19920159033926));
#18663=CARTESIAN_POINT('Ctrl Pts',(-1.55315502041598,-0.91330760001291,
9.1964847376212));
#18664=CARTESIAN_POINT('Ctrl Pts',(-1.58867598518827,-0.853376054373785,
9.19377199178822));
#18665=CARTESIAN_POINT('Ctrl Pts',(-1.6230423285283,-0.795392604669187,
9.19114742471105));
#18666=CARTESIAN_POINT('Ctrl Pts',(-1.65434131270559,-0.735560522670982,
9.18852670186681));
#18667=CARTESIAN_POINT('Ctrl Pts',(-1.68236622824247,-0.674140102529266,
9.1859055831635));
#18668=CARTESIAN_POINT('Ctrl Pts',(-1.69115054831466,-0.654888068431862,
9.18508400189569));
#18669=CARTESIAN_POINT('Ctrl Pts',(-1.69961287778241,-0.63547984453725,
9.18426238173516));
#18670=CARTESIAN_POINT('Ctrl Pts',(-1.70774593841608,-0.615923128385269,
9.18344059210489));
#18671=CARTESIAN_POINT('Ctrl Pts',(-1.71216302078559,-0.605301834629889,
9.18299427642487));
#18672=CARTESIAN_POINT('Ctrl Pts',(-1.71647899938211,-0.594646287471263,
9.18254831195315));
#18673=CARTESIAN_POINT('Ctrl Pts',(-1.72069300111537,-0.583958415385776,
9.18210269794168));
#18674=CARTESIAN_POINT('Ctrl Pts',(-1.7465485778942,-0.518381532697819,
9.17936857298954));
#18675=CARTESIAN_POINT('Ctrl Pts',(-1.76857092720554,-0.451584515773078,
9.17664740083961));
#18676=CARTESIAN_POINT('Ctrl Pts',(-1.78657879748973,-0.383887803013472,
9.17393456255171));
#18677=CARTESIAN_POINT('Ctrl Pts',(-1.804265940182,-0.317396796610095,9.17127004103185));
#18678=CARTESIAN_POINT('Ctrl Pts',(-1.818080791813,-0.250036934098204,9.16861355915858));
#18679=CARTESIAN_POINT('Ctrl Pts',(-1.82780692425633,-0.182090439888411,
9.16596074041796));
#18680=CARTESIAN_POINT('Ctrl Pts',(-1.83203474093648,-0.152555028639186,
9.16480759641274));
#18681=CARTESIAN_POINT('Ctrl Pts',(-1.83548936700523,-0.122908576611995,
9.16365514456446));
#18682=CARTESIAN_POINT('Ctrl Pts',(-1.83814997966601,-0.0931736312707507,
9.16250302540846));
#18683=CARTESIAN_POINT('Ctrl Pts',(-1.84090084649807,-0.0624300074061506,
9.16131182369032));
#18684=CARTESIAN_POINT('Ctrl Pts',(-1.8428029176425,-0.0315917693259644,
9.16012097761867));
#18685=CARTESIAN_POINT('Ctrl Pts',(-1.84387051712372,-0.000685899417074366,
9.15893008989225));
#18686=CARTESIAN_POINT('',(1.57682165668711,1.14877748587887,9.046));
#18687=CARTESIAN_POINT('Ctrl Pts',(1.57638112755701,1.14851130170693,9.046));
#18688=CARTESIAN_POINT('Ctrl Pts',(1.52665365100122,1.20039535614393,9.05556311183685));
#18689=CARTESIAN_POINT('Ctrl Pts',(1.47436073626302,1.24949348117112,9.06516696825537));
#18690=CARTESIAN_POINT('Ctrl Pts',(1.41972944071722,1.2955534749412,9.07483034464178));
#18691=CARTESIAN_POINT('Ctrl Pts',(1.3664938249483,1.3404367621883,9.08424684826298));
#18692=CARTESIAN_POINT('Ctrl Pts',(1.31103689266819,1.38243551265733,9.09371986955463));
#18693=CARTESIAN_POINT('Ctrl Pts',(1.25355103002689,1.42127113207222,9.10326678137301));
#18694=CARTESIAN_POINT('Ctrl Pts',(1.21505546529212,1.44727751055399,9.10965989691543));
#18695=CARTESIAN_POINT('Ctrl Pts',(1.17564971559358,1.4718644964471,9.11608614753966));
#18696=CARTESIAN_POINT('Ctrl Pts',(1.1353897956679,1.4949355025024,9.12255075023748));
#18697=CARTESIAN_POINT('Ctrl Pts',(1.10085612021387,1.5147250757798,9.12809588028041));
#18698=CARTESIAN_POINT('Ctrl Pts',(1.06569392033189,1.53339909402576,9.13366922848017));
#18699=CARTESIAN_POINT('Ctrl Pts',(1.02993870461658,1.55088989389757,9.13927408736756));
#18700=CARTESIAN_POINT('Ctrl Pts',(1.01974786900349,1.55587506494657,9.14087156606859));
#18701=CARTESIAN_POINT('Ctrl Pts',(1.00951092351917,1.56076299370641,9.14247127864936));
#18702=CARTESIAN_POINT('Ctrl Pts',(0.99923854738173,1.56554780312885,9.14407178199195));
#18703=CARTESIAN_POINT('Ctrl Pts',(0.938937254424059,1.59363577331886,9.15346711756474));
#18704=CARTESIAN_POINT('Ctrl Pts',(0.877320674058788,1.61822126093367,9.16290462306444));
#18705=CARTESIAN_POINT('Ctrl Pts',(0.814565971029498,1.6390607692062,9.17240255066083));
#18706=CARTESIAN_POINT('Ctrl Pts',(0.794337488449258,1.64577822000625,9.1754641325608));
#18707=CARTESIAN_POINT('Ctrl Pts',(0.773990691920164,1.65210605100162,9.17853199258413));
#18708=CARTESIAN_POINT('Ctrl Pts',(0.753531412608169,1.65803494195743,9.18160674204658));
#18709=CARTESIAN_POINT('Ctrl Pts',(0.685680963865546,1.67769731157287,9.19180373518681));
#18710=CARTESIAN_POINT('Ctrl Pts',(0.616592242438488,1.69297649589436,9.20207650030987));
#18711=CARTESIAN_POINT('Ctrl Pts',(0.546660605554544,1.70392247702929,9.21244733474057));
#18712=CARTESIAN_POINT('Ctrl Pts',(0.485470423281094,1.71350021052235,9.22152181486743));
#18713=CARTESIAN_POINT('Ctrl Pts',(0.423634394293533,1.7197591669622,9.23067137930796));
#18714=CARTESIAN_POINT('Ctrl Pts',(0.361433447993987,1.72269786116138,9.23991096552778));
#18715=CARTESIAN_POINT('Ctrl Pts',(0.349628912262679,1.72325556844304,9.24166446016352));
#18716=CARTESIAN_POINT('Ctrl Pts',(0.337810284535043,1.72369353857676,9.24342134888598));
#18717=CARTESIAN_POINT('Ctrl Pts',(0.325996288505707,1.72401147004967,9.24517924372526));
#18718=CARTESIAN_POINT('Ctrl Pts',(0.260416164444351,1.72577632466661,9.25493741203347));
#18719=CARTESIAN_POINT('Ctrl Pts',(0.194857285865191,1.72385320378291,9.26474446521909));
#18720=CARTESIAN_POINT('Ctrl Pts',(0.129635755801097,1.71831420943767,9.27462138494297));
#18721=CARTESIAN_POINT('Ctrl Pts',(0.0648376826768893,1.71281117753602,
9.28443417783331));
#18722=CARTESIAN_POINT('Ctrl Pts',(0.00037157230131897,1.70373855506801,
9.29431593297685));
#18723=CARTESIAN_POINT('Ctrl Pts',(-0.0634310656618756,1.69112091958725,
9.3042872260058));
#18724=CARTESIAN_POINT('Ctrl Pts',(-0.125882183323273,1.67877056130784,
9.31404729885022));
#18725=CARTESIAN_POINT('Ctrl Pts',(-0.187698423459061,1.66302322279157,
9.32389315642556));
#18726=CARTESIAN_POINT('Ctrl Pts',(-0.248535080977911,1.64386571170743,
9.33384409431584));
#18727=CARTESIAN_POINT('Ctrl Pts',(-0.264799294326261,1.63874409819013,
9.33650440116806));
#18728=CARTESIAN_POINT('Ctrl Pts',(-0.280993269093027,1.63337857463901,
9.3391722183119));
#18729=CARTESIAN_POINT('Ctrl Pts',(-0.2971098906338,1.62776851541254,9.34184791443712));
#18730=CARTESIAN_POINT('Ctrl Pts',(-0.307118321623271,1.62428466549568,
9.34350952322718));
#18731=CARTESIAN_POINT('Ctrl Pts',(-0.317095956597471,1.62070676207948,
9.34517401751648));
#18732=CARTESIAN_POINT('Ctrl Pts',(-0.327029564295253,1.61703917202283,
9.34683953674638));
#18733=CARTESIAN_POINT('Ctrl Pts',(-0.385058843550973,1.59561416571415,
9.35656902108263));
#18734=CARTESIAN_POINT('Ctrl Pts',(-0.441695945414057,1.57109483599993,
9.36635131878856));
#18735=CARTESIAN_POINT('Ctrl Pts',(-0.496653381265967,1.54351374113654,
9.37620782348998));
#18736=CARTESIAN_POINT('Ctrl Pts',(-0.550666441336512,1.51640659338528,
9.38589495630962));
#18737=CARTESIAN_POINT('Ctrl Pts',(-0.603057746949111,1.48634144533044,
9.39565376772527));
#18738=CARTESIAN_POINT('Ctrl Pts',(-0.653517363153777,1.45331593243132,
9.40550456733641));
#18739=CARTESIAN_POINT('Ctrl Pts',(-0.702505928279116,1.4212532135455,9.4150681862179));
#18740=CARTESIAN_POINT('Ctrl Pts',(-0.749674214490309,1.38639968870215,
9.42471850800499));
#18741=CARTESIAN_POINT('Ctrl Pts',(-0.794695568814028,1.3487295473085,9.43447411731777));
#18742=CARTESIAN_POINT('Ctrl Pts',(-0.810060718838732,1.33587326204877,
9.43780356848434));
#18743=CARTESIAN_POINT('Ctrl Pts',(-0.825175397375936,1.32268873629785,
9.44114528312221));
#18744=CARTESIAN_POINT('Ctrl Pts',(-0.840025297123196,1.30917445368946,
9.4445));
#18745=CARTESIAN_POINT('',(0.0562002947523052,1.95126002955752,9.046));
#18746=CARTESIAN_POINT('Origin',(0.,0.,9.046));
#18747=CARTESIAN_POINT('Ctrl Pts',(-1.84387051712372,-0.000685899417074366,
9.15893008989225));
#18748=CARTESIAN_POINT('Ctrl Pts',(-1.84476283066793,0.0251456289795263,
9.15793473042775));
#18749=CARTESIAN_POINT('Ctrl Pts',(-1.84507215638603,0.0510244107480692,
9.15693934186537));
#18750=CARTESIAN_POINT('Ctrl Pts',(-1.84480573917948,0.0769346286138066,
9.1559436922441));
#18751=CARTESIAN_POINT('Ctrl Pts',(-1.84407856754811,0.147655193694427,
9.15322611942388));
#18752=CARTESIAN_POINT('Ctrl Pts',(-1.83907076887915,0.218209205892797,
9.15052194970773));
#18753=CARTESIAN_POINT('Ctrl Pts',(-1.83003406491836,0.288270461308813,
9.14782667059928));
#18754=CARTESIAN_POINT('Ctrl Pts',(-1.82102660530416,0.35810498631012,9.14514011388306));
#18755=CARTESIAN_POINT('Ctrl Pts',(-1.80801584752918,0.427450903626474,
9.14246239032455));
#18756=CARTESIAN_POINT('Ctrl Pts',(-1.79119418439719,0.495991519692167,
9.13978903109544));
#18757=CARTESIAN_POINT('Ctrl Pts',(-1.77853014929814,0.54759169505862,9.13777641707242));
#18758=CARTESIAN_POINT('Ctrl Pts',(-1.76370501453111,0.598735674972647,
9.13576627661749));
#18759=CARTESIAN_POINT('Ctrl Pts',(-1.74678162412797,0.649285717226304,
9.13375670293922));
#18760=CARTESIAN_POINT('Ctrl Pts',(-1.73714767088699,0.678062264466551,
9.13261271592541));
#18761=CARTESIAN_POINT('Ctrl Pts',(-1.72683345109667,0.7066462701884,9.131468912585));
#18762=CARTESIAN_POINT('Ctrl Pts',(-1.71584835159382,0.735011504504436,
9.13032494115134));
#18763=CARTESIAN_POINT('Ctrl Pts',(-1.71100614127397,0.747514844168743,
9.12982068078663));
#18764=CARTESIAN_POINT('Ctrl Pts',(-1.70603355688525,0.75997566624557,9.12931638776091));
#18765=CARTESIAN_POINT('Ctrl Pts',(-1.70093130867429,0.772391673509186,
9.12881203194595));
#18766=CARTESIAN_POINT('Ctrl Pts',(-1.69655013131485,0.783052999197183,
9.12837895378388));
#18767=CARTESIAN_POINT('Ctrl Pts',(-1.69207380809,0.79367997378185,9.12794588138746));
#18768=CARTESIAN_POINT('Ctrl Pts',(-1.68750792088798,0.804259883490199,
9.12751325944918));
#18769=CARTESIAN_POINT('Ctrl Pts',(-1.65901258128147,0.8702882601905,9.12481330027211));
#18770=CARTESIAN_POINT('Ctrl Pts',(-1.62698410576056,0.934604514869337,
9.12212599867707));
#18771=CARTESIAN_POINT('Ctrl Pts',(-1.59161919700648,0.996889483350542,
9.11944691608334));
#18772=CARTESIAN_POINT('Ctrl Pts',(-1.55617870750904,1.05930756525925,9.11676210784062));
#18773=CARTESIAN_POINT('Ctrl Pts',(-1.51738711621801,1.11968666473227,9.11408555376753));
#18774=CARTESIAN_POINT('Ctrl Pts',(-1.47539333726015,1.17769038855139,9.11141278676449));
#18775=CARTESIAN_POINT('Ctrl Pts',(-1.43413146740691,1.23468316611567,9.10878660338771));
#18776=CARTESIAN_POINT('Ctrl Pts',(-1.38977757023931,1.2893835170435,9.10616407622178));
#18777=CARTESIAN_POINT('Ctrl Pts',(-1.34243235737242,1.34144399157684,9.10354096769098));
#18778=CARTESIAN_POINT('Ctrl Pts',(-1.32721791009383,1.35817369447865,9.1026980282673));
#18779=CARTESIAN_POINT('Ctrl Pts',(-1.31169427190245,1.37463051052086,9.101855028808));
#18780=CARTESIAN_POINT('Ctrl Pts',(-1.2958639972742,1.39080204565998,9.10101182868962));
#18781=CARTESIAN_POINT('Ctrl Pts',(-1.28762458675722,1.39921907693897,9.10057295620721));
#18782=CARTESIAN_POINT('Ctrl Pts',(-1.27930873672108,1.40755201990811,9.10013438322948));
#18783=CARTESIAN_POINT('Ctrl Pts',(-1.27091852207937,1.41579817729257,9.0996961596087));
#18784=CARTESIAN_POINT('Ctrl Pts',(-1.22163456203449,1.46423594776861,9.09712204245684));
#18785=CARTESIAN_POINT('Ctrl Pts',(-1.16977311651428,1.50969609064883,9.09455919964471));
#18786=CARTESIAN_POINT('Ctrl Pts',(-1.11547064510272,1.55188751878994,9.09200378176057));
#18787=CARTESIAN_POINT('Ctrl Pts',(-1.05997608101023,1.59500516799204,9.08939226523345));
#18788=CARTESIAN_POINT('Ctrl Pts',(-1.00193205212083,1.63471019377729,9.08678850320891));
#18789=CARTESIAN_POINT('Ctrl Pts',(-0.941699156915238,1.67101078688361,
9.08418838715268));
#18790=CARTESIAN_POINT('Ctrl Pts',(-0.880245158955871,1.70804730267893,
9.08153555888884));
#18791=CARTESIAN_POINT('Ctrl Pts',(-0.816511792195639,1.74154029826807,
9.07888652592138));
#18792=CARTESIAN_POINT('Ctrl Pts',(-0.750851384302144,1.7714536219802,9.07623692473885));
#18793=CARTESIAN_POINT('Ctrl Pts',(-0.735368379689796,1.77850731146925,
9.07561213746375));
#18794=CARTESIAN_POINT('Ctrl Pts',(-0.719778125572124,1.78536175208163,
9.07498731859381));
#18795=CARTESIAN_POINT('Ctrl Pts',(-0.704085082311001,1.79201608287082,
9.07436241091651));
#18796=CARTESIAN_POINT('Ctrl Pts',(-0.689155208372567,1.79834680650256,
9.07376789316174));
#18797=CARTESIAN_POINT('Ctrl Pts',(-0.674127745726515,1.80449806819125,
9.07317311800809));
#18798=CARTESIAN_POINT('Ctrl Pts',(-0.659034674467403,1.81045829022041,
9.07257913841047));
#18799=CARTESIAN_POINT('Ctrl Pts',(-0.591575493283209,1.83709777868902,
9.0699243190826));
#18800=CARTESIAN_POINT('Ctrl Pts',(-0.522714141676951,1.85996688588042,
9.06728160073073));
#18801=CARTESIAN_POINT('Ctrl Pts',(-0.452831713589392,1.87908057169854,
9.064646767212));
#18802=CARTESIAN_POINT('Ctrl Pts',(-0.381964429865557,1.8984636273958,9.06197480088732));
#18803=CARTESIAN_POINT('Ctrl Pts',(-0.310046121550136,1.91398495893907,
9.05931094320431));
#18804=CARTESIAN_POINT('Ctrl Pts',(-0.237448384653525,1.92561288101988,
9.05665079724139));
#18805=CARTESIAN_POINT('Ctrl Pts',(-0.16509915768935,1.93720099946144,9.0539997572468));
#18806=CARTESIAN_POINT('Ctrl Pts',(-0.0920741051298766,1.94492250064192,
9.05135240360455));
#18807=CARTESIAN_POINT('Ctrl Pts',(-0.0187307257833482,1.94869601579968,
9.04870438439208));
#18808=CARTESIAN_POINT('Ctrl Pts',(0.00623373766317573,1.94998043686209,
9.04780305724539));
#18809=CARTESIAN_POINT('Ctrl Pts',(0.0312350991919573,1.95080701502899,
9.04690165298766));
#18810=CARTESIAN_POINT('Ctrl Pts',(0.0562592026297113,1.95117115182352,
9.046));
#18811=CARTESIAN_POINT('',(-1.,-1.22464679914735E-16,10.));
#18812=CARTESIAN_POINT('',(-1.5,-1.83697019872103E-16,9.5));
#18813=CARTESIAN_POINT('Origin',(0.,0.,10.));
#18814=CARTESIAN_POINT('Ctrl Pts',(1.13509973994372,-1.59049193030952,-0.230074082272068));
#18815=CARTESIAN_POINT('Ctrl Pts',(1.6638518199518,-1.21313299055364,-0.193036827370107));
#18816=CARTESIAN_POINT('Ctrl Pts',(2.3063342838214,0.103787718385998,-0.118962317566186));
#18817=CARTESIAN_POINT('Ctrl Pts',(1.16188726092372,1.99754004216699,-0.0078505528603034));
#18818=CARTESIAN_POINT('Ctrl Pts',(-1.04656155408942,2.05782827558088,0.103261211845579));
#18819=CARTESIAN_POINT('Ctrl Pts',(-2.29698247648793,0.238323790666827,
0.214372976551461));
#18820=CARTESIAN_POINT('Ctrl Pts',(-1.44612258918391,-1.80076047995977,
0.325484741257344));
#18821=CARTESIAN_POINT('Ctrl Pts',(0.727960807006611,-2.19149445634993,
0.436596505963226));
#18822=CARTESIAN_POINT('Ctrl Pts',(2.23594625441705,-0.57761383484556,0.547708270669108));
#18823=CARTESIAN_POINT('Ctrl Pts',(1.69826458517493,1.56495710236821,0.658820035374991));
#18824=CARTESIAN_POINT('Ctrl Pts',(-0.393209187557514,2.27560539746713,
0.769931800080872));
#18825=CARTESIAN_POINT('Ctrl Pts',(-2.1249183445612,0.904323940984954,0.881043564786756));
#18826=CARTESIAN_POINT('Ctrl Pts',(-1.91250851401755,-1.29437122529363,
0.992155329492637));
#18827=CARTESIAN_POINT('Ctrl Pts',(0.0496914524290519,-2.30880688864344,
1.10326709419852));
#18828=CARTESIAN_POINT('Ctrl Pts',(1.96642629593332,-1.21088396446372,1.2143788589044));
#18829=CARTESIAN_POINT('Ctrl Pts',(2.08404446099042,0.994902325724329,1.32549062361028));
#18830=CARTESIAN_POINT('Ctrl Pts',(0.294933807152522,2.29043279904655,1.43660238831617));
#18831=CARTESIAN_POINT('Ctrl Pts',(-1.76401667284967,1.49040789535707,1.54771415302205));
#18832=CARTESIAN_POINT('Ctrl Pts',(-2.20903784902227,-0.673217691022686,
1.65882591772793));
#18833=CARTESIAN_POINT('Ctrl Pts',(-0.632971955670129,-2.22090439277293,
1.76993768243381));
#18834=CARTESIAN_POINT('Ctrl Pts',(1.52221091586757,-1.73664736597321,1.8810494471397));
#18835=CARTESIAN_POINT('Ctrl Pts',(2.28469665983849,0.336498526979157,1.99216121184558));
#18836=CARTESIAN_POINT('Ctrl Pts',(0.956873830222989,2.10177603540478,2.10327297655146));
#18837=CARTESIAN_POINT('Ctrl Pts',(-1.24640944320213,1.94410225513366,2.21438474125735));
#18838=CARTESIAN_POINT('Ctrl Pts',(-2.30933112102653,0.0077356190240744,
2.32549650596323));
#18839=CARTESIAN_POINT('Ctrl Pts',(-1.25940573752146,-1.93570846156897,
2.43660827066911));
#18840=CARTESIAN_POINT('Ctrl Pts',(0.942771778257433,-2.10813933150712,
2.54772003537499));
#18841=CARTESIAN_POINT('Ctrl Pts',(2.28239105758209,-0.351796993969821,
2.65883180008088));
#18842=CARTESIAN_POINT('Ctrl Pts',(1.5338112075673,1.72641050841568,2.76994356478675));
#18843=CARTESIAN_POINT('Ctrl Pts',(-0.618079094904134,2.22509512099281,
2.88105532949264));
#18844=CARTESIAN_POINT('Ctrl Pts',(-2.20447812307392,0.688001649364983,
2.99216709419852));
#18845=CARTESIAN_POINT('Ctrl Pts',(-1.77396191596644,-1.47855645319501,
3.1032788589044));
#18846=CARTESIAN_POINT('Ctrl Pts',(0.279582788264576,-2.29235763554206,
3.21439062361029));
#18847=CARTESIAN_POINT('Ctrl Pts',(2.07733235475043,-1.00884109381303,3.32550238831616));
#18848=CARTESIAN_POINT('Ctrl Pts',(1.97449455267563,1.19768164639481,3.43661415302206));
#18849=CARTESIAN_POINT('Ctrl Pts',(0.0651574691963124,2.30842469421968,
3.54772591772793));
#18850=CARTESIAN_POINT('Ctrl Pts',(-1.90379331193745,1.30714998760185,3.65883768243382));
#18851=CARTESIAN_POINT('Ctrl Pts',(-2.13093060196669,-0.890058893707459,
3.7699494471397));
#18852=CARTESIAN_POINT('Ctrl Pts',(-0.408442558280485,-2.27293746971921,
3.88106121184558));
#18853=CARTESIAN_POINT('Ctrl Pts',(1.68773665970145,-1.57626616793184,3.99217297655146));
#18854=CARTESIAN_POINT('Ctrl Pts',(2.23977636166251,0.562558365331801,4.10328474125734));
#18855=CARTESIAN_POINT('Ctrl Pts',(0.74260585822099,2.18668850182259,4.21439650596323));
#18856=CARTESIAN_POINT('Ctrl Pts',(-1.43398761320325,1.81017943581477,4.32550827066911));
#18857=CARTESIAN_POINT('Ctrl Pts',(-2.29860096835557,-0.222494163837853,
4.43662003537499));
#18858=CARTESIAN_POINT('Ctrl Pts',(-1.06018446609557,-2.05160399748995,
4.54773180008088));
#18859=CARTESIAN_POINT('Ctrl Pts',(1.14821317567414,-2.00366578247853,4.65884356478675));
#18860=CARTESIAN_POINT('Ctrl Pts',(2.30609068612924,-0.122539022418222,
4.76995532949264));
#18861=CARTESIAN_POINT('Ctrl Pts',(1.35408586659467,1.87070081267837,4.88106709419852));
#18862=CARTESIAN_POINT('Ctrl Pts',(-0.836795576656505,2.15240405768872,
4.99217885890441));
#18863=CARTESIAN_POINT('Ctrl Pts',(-2.26207824635583,0.464835532239094,
5.10329062361028));
#18864=CARTESIAN_POINT('Ctrl Pts',(-1.61774632988599,-1.64801907659051,
5.21440238831616));
#18865=CARTESIAN_POINT('Ctrl Pts',(0.506689737022565,-2.25307247443603,
5.32551415302206));
#18866=CARTESIAN_POINT('Ctrl Pts',(2.16754658332471,-0.796750822900503,
5.43662591772793));
#18867=CARTESIAN_POINT('Ctrl Pts',(1.84527750005797,1.38853196305901,5.54773768243382));
#18868=CARTESIAN_POINT('Ctrl Pts',(-0.165267944017207,2.30342279474246,
5.65884944713968));
#18869=CARTESIAN_POINT('Ctrl Pts',(-2.02460688227655,1.11087219650157,5.76996121184559));
#18870=CARTESIAN_POINT('Ctrl Pts',(-2.03159790035992,-1.09803462415223,
5.88107297655145));
#18871=CARTESIAN_POINT('Ctrl Pts',(-0.179844794802175,-2.30233053978421,
5.99218474125735));
#18872=CARTESIAN_POINT('Ctrl Pts',(1.83645143012731,-1.40018434850804,6.10329650596322));
#18873=CARTESIAN_POINT('Ctrl Pts',(2.17254641826527,0.783014766469867,6.21440827066911));
#18874=CARTESIAN_POINT('Ctrl Pts',(0.520941041773343,2.24982010296223,6.32552003537499));
#18875=CARTESIAN_POINT('Ctrl Pts',(-1.60728232206565,1.65822604131681,6.43663180008087));
#18876=CARTESIAN_POINT('Ctrl Pts',(-2.26497523551502,-0.450507760638336,
6.54774356478676));
#18877=CARTESIAN_POINT('Ctrl Pts',(-0.850403061079838,-2.14706420492014,
6.65885532949263));
#18878=CARTESIAN_POINT('Ctrl Pts',(1.34221761756673,-1.87923440411587,6.76996709419852));
#18879=CARTESIAN_POINT('Ctrl Pts',(2.30682012517322,0.107939520395821,6.8810788589044));
#18880=CARTESIAN_POINT('Ctrl Pts',(1.16087295306313,1.99635770166139,6.99219062361028));
#18881=CARTESIAN_POINT('Ctrl Pts',(-1.04717705090239,2.05827363831718,7.10330238831617));
#18882=CARTESIAN_POINT('Ctrl Pts',(-2.29714652812405,0.237039336040665,
7.21441415302205));
#18883=CARTESIAN_POINT('Ctrl Pts',(-1.44541702482095,-1.80106632367513,
7.32552591772793));
#18884=CARTESIAN_POINT('Ctrl Pts',(0.728749912475137,-2.19134526757008,
7.43663768243382));
#18885=CARTESIAN_POINT('Ctrl Pts',(2.23617025832252,-0.576724313119789,
7.54774944713969));
#18886=CARTESIAN_POINT('Ctrl Pts',(1.69768095784581,1.56555144229893,7.65886121184558));
#18887=CARTESIAN_POINT('Ctrl Pts',(-0.394048492723434,2.27547756264829,
7.76997297655146));
#18888=CARTESIAN_POINT('Ctrl Pts',(-2.1252515343864,0.903528862339296,7.88108474125734));
#18889=CARTESIAN_POINT('Ctrl Pts',(-1.91203390686379,-1.29507220804901,
7.99219650596323));
#18890=CARTESIAN_POINT('Ctrl Pts',(0.0505534074973998,-2.30879278288063,
8.10330827066911));
#18891=CARTESIAN_POINT('Ctrl Pts',(1.9668566708909,-1.21015215007583,8.21442003537499));
#18892=CARTESIAN_POINT('Ctrl Pts',(2.08370935603324,0.995664930130442,8.32553180008088));
#18893=CARTESIAN_POINT('Ctrl Pts',(0.294024709520203,2.2905551434179,8.43664356478675));
#18894=CARTESIAN_POINT('Ctrl Pts',(-1.76444823276047,1.48973062083675,8.54775532949265));
#18895=CARTESIAN_POINT('Ctrl Pts',(-2.20901589213136,-0.673986377788178,
8.65886709419851));
#18896=CARTESIAN_POINT('Ctrl Pts',(-0.631718430347985,-2.22122906321008,
8.76997885890441));
#18897=CARTESIAN_POINT('Ctrl Pts',(1.52202596973473,-1.73591049473505,8.88109062361028));
#18898=CARTESIAN_POINT('Ctrl Pts',(2.28617112150847,0.33700123195322,8.99220238831617));
#18899=CARTESIAN_POINT('Ctrl Pts',(0.952838501929636,2.10286673578195,9.10331415302205));
#18900=CARTESIAN_POINT('Ctrl Pts',(-0.508499740558942,1.99537528935738,
9.17738866282597));
#18901=CARTESIAN_POINT('Ctrl Pts',(-1.05522946356713,1.64456887335855,9.21442591772793));
#18902=CARTESIAN_POINT('Ctrl Pts',(1.05793541951255,-1.48236995244729,-0.153382721514713));
#18903=CARTESIAN_POINT('Ctrl Pts',(1.55074282127375,-1.13066395323947,-0.116345466612752));
#18904=CARTESIAN_POINT('Ctrl Pts',(2.14954919134395,0.0967322073357151,
-0.0422709568088308));
#18905=CARTESIAN_POINT('Ctrl Pts',(1.08290191914989,1.86174684755704,0.0688408078970521));
#18906=CARTESIAN_POINT('Ctrl Pts',(-0.975416078261274,1.91793667411056,
0.179952572602934));
#18907=CARTESIAN_POINT('Ctrl Pts',(-2.14083312185121,0.222122488964202,
0.291064337308817));
#18908=CARTESIAN_POINT('Ctrl Pts',(-1.34781486967012,-1.67834440161383,
0.402176102014699));
#18909=CARTESIAN_POINT('Ctrl Pts',(0.678473877359381,-2.04251619963627,
0.513287866720582));
#18910=CARTESIAN_POINT('Ctrl Pts',(2.08394615506782,-0.538347524168997,
0.624399631426463));
#18911=CARTESIAN_POINT('Ctrl Pts',(1.5828161994376,1.45857098751088,0.735511396132347));
#18912=CARTESIAN_POINT('Ctrl Pts',(-0.366478743811078,2.12090926118418,
0.846623160838227));
#18913=CARTESIAN_POINT('Ctrl Pts',(-1.98046594600992,0.842847808183427,
0.957734925544112));
#18914=CARTESIAN_POINT('Ctrl Pts',(-1.78249578067807,-1.20637959559737,
1.06884669024999));
#18915=CARTESIAN_POINT('Ctrl Pts',(0.0463134169816076,-2.15185370796715,
1.17995845495588));
#18916=CARTESIAN_POINT('Ctrl Pts',(1.83274822037389,-1.12856781641888,1.29107021966175));
#18917=CARTESIAN_POINT('Ctrl Pts',(1.9423706776904,0.927268655168022,1.40218198436764));
#18918=CARTESIAN_POINT('Ctrl Pts',(0.274884144554374,2.13472869286777,1.51329374907352));
#18919=CARTESIAN_POINT('Ctrl Pts',(-1.64409844628356,1.38908965136187,1.62440551377941));
#18920=CARTESIAN_POINT('Ctrl Pts',(-2.05886698876376,-0.627452209979957,
1.73551727848529));
#18921=CARTESIAN_POINT('Ctrl Pts',(-0.589942388229901,-2.06992684236011,
1.84662904319117));
#18922=CARTESIAN_POINT('Ctrl Pts',(1.41873069581074,-1.61858971067802,1.95774080789705));
#18923=CARTESIAN_POINT('Ctrl Pts',(2.12938249761644,0.313623285934951,2.06885257260293));
#18924=CARTESIAN_POINT('Ctrl Pts',(0.891825344835078,1.95889685592529,2.17996433730882));
#18925=CARTESIAN_POINT('Ctrl Pts',(-1.1616782655979,1.81194177259002,2.2910761020147));
#18926=CARTESIAN_POINT('Ctrl Pts',(-2.15234230292194,0.00720975000647539,
2.40218786672058));
#18927=CARTESIAN_POINT('Ctrl Pts',(-1.17379106908025,-1.80411859088743,
2.51329963142647));
#18928=CARTESIAN_POINT('Ctrl Pts',(0.878681953345199,-1.96482757381254,
2.62441139613234));
#18929=CARTESIAN_POINT('Ctrl Pts',(2.12723363068914,-0.327881759903454,
2.73552316083823));
#18930=CARTESIAN_POINT('Ctrl Pts',(1.42954239722687,1.60904875686269,2.84663492554411));
#18931=CARTESIAN_POINT('Ctrl Pts',(-0.576061947289118,2.07383268398912,
2.95774669024999));
#18932=CARTESIAN_POINT('Ctrl Pts',(-2.05461723394991,0.641231151706844,
3.06885845495588));
#18933=CARTESIAN_POINT('Ctrl Pts',(-1.6533676096695,-1.37804387274497,3.17997021966176));
#18934=CARTESIAN_POINT('Ctrl Pts',(0.260576691177686,-2.13652267857115,
3.29108198436765));
#18935=CARTESIAN_POINT('Ctrl Pts',(1.93611486185244,-0.94025986285354,3.40219374907351));
#18936=CARTESIAN_POINT('Ctrl Pts',(1.84026799531615,1.11626299472502,3.51330551377941));
#18937=CARTESIAN_POINT('Ctrl Pts',(0.0607280506574504,2.15149749520116,
3.62441727848528));
#18938=CARTESIAN_POINT('Ctrl Pts',(-1.77437303987893,1.21828965494074,3.73552904319117));
#18939=CARTESIAN_POINT('Ctrl Pts',(-1.98606948888519,-0.829552501837387,
3.84664080789705));
#18940=CARTESIAN_POINT('Ctrl Pts',(-0.380676546769933,-2.11842269972892,
3.95775257260293));
#18941=CARTESIAN_POINT('Ctrl Pts',(1.57300396456481,-1.46911126040525,4.06886433730882));
#18942=CARTESIAN_POINT('Ctrl Pts',(2.08751589081254,0.524315528657517,4.1799761020147));
#18943=CARTESIAN_POINT('Ctrl Pts',(0.692123354894286,2.03803695491432,4.29108786672059));
#18944=CARTESIAN_POINT('Ctrl Pts',(-1.33650483192358,1.68712305485737,4.40219963142646));
#18945=CARTESIAN_POINT('Ctrl Pts',(-2.14234158829933,-0.207368963515553,
4.51331139613235));
#18946=CARTESIAN_POINT('Ctrl Pts',(-0.988112901827546,-1.9121355237609,
4.62442316083823));
#18947=CARTESIAN_POINT('Ctrl Pts',(1.07015740110811,-1.86745615874641,4.73553492554411));
#18948=CARTESIAN_POINT('Ctrl Pts',(2.14932215347443,-0.114208793753307,
4.84664669024999));
#18949=CARTESIAN_POINT('Ctrl Pts',(1.2620348229512,1.7435301757196,4.95775845495587));
#18950=CARTESIAN_POINT('Ctrl Pts',(-0.779910036346446,2.00608317454491,
5.06887021966176));
#18951=CARTESIAN_POINT('Ctrl Pts',(-2.10830168866686,0.433235914429924,
5.17998198436764));
#18952=CARTESIAN_POINT('Ctrl Pts',(-1.50777159217538,-1.53598639115529,
5.29109374907352));
#18953=CARTESIAN_POINT('Ctrl Pts',(0.472244861518737,-2.09990813102716,
5.40220551377941));
#18954=CARTESIAN_POINT('Ctrl Pts',(2.02019630808506,-0.742587533421502,
5.51331727848529));
#18955=CARTESIAN_POINT('Ctrl Pts',(1.71983514526896,1.29413926649146,5.62442904319117));
#18956=CARTESIAN_POINT('Ctrl Pts',(-0.154032994223487,2.14683562590847,
5.73554080789705));
#18957=CARTESIAN_POINT('Ctrl Pts',(-1.88697367815045,1.03535486959847,5.84665257260293));
#18958=CARTESIAN_POINT('Ctrl Pts',(-1.89348944534568,-1.02338999813302,
5.95776433730882));
#18959=CARTESIAN_POINT('Ctrl Pts',(-0.1676189076086,-2.14581762267332,6.06887610201469));
#18960=CARTESIAN_POINT('Ctrl Pts',(1.7116090734392,-1.3049995203128,6.17998786672059));
#18961=CARTESIAN_POINT('Ctrl Pts',(2.02485625318872,0.729785257012656,6.29109963142646));
#18962=CARTESIAN_POINT('Ctrl Pts',(0.485527359557932,2.09687685645413,6.40221139613235));
#18963=CARTESIAN_POINT('Ctrl Pts',(-1.49801892982015,1.54549948426039,6.51332316083823));
#18964=CARTESIAN_POINT('Ctrl Pts',(-2.11100173989019,-0.419882147773394,
6.62443492554411));
#18965=CARTESIAN_POINT('Ctrl Pts',(-0.792592481100246,-2.0011063260971,
6.73554669024999));
#18966=CARTESIAN_POINT('Ctrl Pts',(1.25097338000271,-1.75148365180605,6.84665845495587));
#18967=CARTESIAN_POINT('Ctrl Pts',(2.15000200509789,0.100601768966674,6.95777021966176));
#18968=CARTESIAN_POINT('Ctrl Pts',(1.08195656415223,1.86064488280912,7.06888198436763));
#18969=CARTESIAN_POINT('Ctrl Pts',(-0.975989733470706,1.91835176099384,
7.17999374907353));
#18970=CARTESIAN_POINT('Ctrl Pts',(-2.14098602122241,0.220925351835228,
7.2911055137794));
#18971=CARTESIAN_POINT('Ctrl Pts',(-1.3471572697218,-1.67862945400872,7.40221727848529));
#18972=CARTESIAN_POINT('Ctrl Pts',(0.679209339271233,-2.04237715274123,
7.51332904319116));
#18973=CARTESIAN_POINT('Ctrl Pts',(2.08415493114041,-0.537518472318304,
7.62444080789706));
#18974=CARTESIAN_POINT('Ctrl Pts',(1.58227224721776,1.45912492408739,7.73555257260292));
#18975=CARTESIAN_POINT('Ctrl Pts',(-0.36726099283428,2.12079011660337,7.84666433730883));
#18976=CARTESIAN_POINT('Ctrl Pts',(-1.98077648552032,0.842106779152281,
7.95777610201469));
#18977=CARTESIAN_POINT('Ctrl Pts',(-1.78205343741902,-1.20703292539676,
8.0688878667206));
#18978=CARTESIAN_POINT('Ctrl Pts',(0.047116776162082,-2.15184056111708,
8.17999963142645));
#18979=CARTESIAN_POINT('Ctrl Pts',(1.83314933835081,-1.12788575092788,8.29111139613235));
#18980=CARTESIAN_POINT('Ctrl Pts',(1.9420583532391,0.92797941756529,8.40222316083823));
#18981=CARTESIAN_POINT('Ctrl Pts',(0.2740368475714,2.13484272024287,8.51333492554411));
#18982=CARTESIAN_POINT('Ctrl Pts',(-1.64450066866033,1.38845841810671,8.62444669025));
#18983=CARTESIAN_POINT('Ctrl Pts',(-2.05884652450694,-0.62816864125653,
8.73555845495587));
#18984=CARTESIAN_POINT('Ctrl Pts',(-0.588774077824317,-2.07022944163225,
8.84667021966176));
#18985=CARTESIAN_POINT('Ctrl Pts',(1.41855832235513,-1.61790293210251,8.95778198436763));
#18986=CARTESIAN_POINT('Ctrl Pts',(2.1307567250702,0.31409181691854,9.06889374907353));
#18987=CARTESIAN_POINT('Ctrl Pts',(0.888064339012712,1.9599134102601,9.1800055137794));
#18988=CARTESIAN_POINT('Ctrl Pts',(-0.473931820631839,1.85972925510133,
9.25408002358333));
#18989=CARTESIAN_POINT('Ctrl Pts',(-0.983494741419154,1.53277073346885,
9.29111727848529));
#18990=CARTESIAN_POINT('Ctrl Pts',(0.980771099081378,-1.37424797458506,
-0.0766913607573575));
#18991=CARTESIAN_POINT('Ctrl Pts',(1.43763382259569,-1.0481949159253,-0.0396541058553967));
#18992=CARTESIAN_POINT('Ctrl Pts',(1.99276409886649,0.0896766962854344,
0.0344204039485245));
#18993=CARTESIAN_POINT('Ctrl Pts',(1.00391657737607,1.72595365294709,0.145532168654408));
#18994=CARTESIAN_POINT('Ctrl Pts',(-0.904270602433131,1.77804507264024,
0.256643933360289));
#18995=CARTESIAN_POINT('Ctrl Pts',(-1.9846837672145,0.205921187261574,0.367755698066172));
#18996=CARTESIAN_POINT('Ctrl Pts',(-1.24950715015633,-1.55592832326788,
0.478867462772054));
#18997=CARTESIAN_POINT('Ctrl Pts',(0.628986947712151,-1.89353794292261,
0.589979227477937));
#18998=CARTESIAN_POINT('Ctrl Pts',(1.93194605571859,-0.499081213492431,
0.701090992183818));
#18999=CARTESIAN_POINT('Ctrl Pts',(1.46736781370027,1.35218487265355,0.812202756889702));
#19000=CARTESIAN_POINT('Ctrl Pts',(-0.339748300064645,1.96621312490123,
0.923314521595583));
#19001=CARTESIAN_POINT('Ctrl Pts',(-1.83601354745863,0.781371675381896,
1.03442628630147));
#19002=CARTESIAN_POINT('Ctrl Pts',(-1.65248304733859,-1.11838796590112,
1.14553805100735));
#19003=CARTESIAN_POINT('Ctrl Pts',(0.0429353815341671,-1.99490052729086,
1.25664981571323));
#19004=CARTESIAN_POINT('Ctrl Pts',(1.69907014481445,-1.04625166837404,1.36776158041911));
#19005=CARTESIAN_POINT('Ctrl Pts',(1.80069689439038,0.859634984611714,1.47887334512499));
#19006=CARTESIAN_POINT('Ctrl Pts',(0.254834481956223,1.97902458668898,1.58998510983088));
#19007=CARTESIAN_POINT('Ctrl Pts',(-1.52418021971745,1.28777140736668,1.70109687453676));
#19008=CARTESIAN_POINT('Ctrl Pts',(-1.90869612850525,-0.58168672893723,
1.81220863924264));
#19009=CARTESIAN_POINT('Ctrl Pts',(-0.546912820789672,-1.91894929194728,
1.92332040394852));
#19010=CARTESIAN_POINT('Ctrl Pts',(1.3152504757539,-1.50053205538284,2.03443216865441));
#19011=CARTESIAN_POINT('Ctrl Pts',(1.97406833539439,0.290748044890748,2.14554393336029));
#19012=CARTESIAN_POINT('Ctrl Pts',(0.826776859447168,1.8160176764458,2.25665569806617));
#19013=CARTESIAN_POINT('Ctrl Pts',(-1.07694708799367,1.67978129004639,2.36776746277206));
#19014=CARTESIAN_POINT('Ctrl Pts',(-1.99535348481736,0.00668388098887723,
2.47887922747793));
#19015=CARTESIAN_POINT('Ctrl Pts',(-1.08817640063904,-1.67252872020589,
2.58999099218382));
#19016=CARTESIAN_POINT('Ctrl Pts',(0.814592128432962,-1.82151581611796,
2.70110275688969));
#19017=CARTESIAN_POINT('Ctrl Pts',(1.97207620379619,-0.303966525837088,
2.81221452159559));
#19018=CARTESIAN_POINT('Ctrl Pts',(1.32527358688643,1.49168700530971,2.92332628630146));
#19019=CARTESIAN_POINT('Ctrl Pts',(-0.5340447996741,1.92257024698542,3.03443805100735));
#19020=CARTESIAN_POINT('Ctrl Pts',(-1.9047563448259,0.594460654048706,3.14554981571323));
#19021=CARTESIAN_POINT('Ctrl Pts',(-1.53277330337256,-1.27753129229492,
3.25666158041911));
#19022=CARTESIAN_POINT('Ctrl Pts',(0.241570594090793,-1.98068772160023,
3.367773345125));
#19023=CARTESIAN_POINT('Ctrl Pts',(1.79489736895445,-0.871678631894047,
3.47888510983087));
#19024=CARTESIAN_POINT('Ctrl Pts',(1.70604143795667,1.03484434305524,3.58999687453676));
#19025=CARTESIAN_POINT('Ctrl Pts',(0.0562986321185907,1.99457029618264,
3.70110863924264));
#19026=CARTESIAN_POINT('Ctrl Pts',(-1.64495276782042,1.12942932227964,3.81222040394853));
#19027=CARTESIAN_POINT('Ctrl Pts',(-1.84120837580369,-0.769046109967315,
3.92333216865441));
#19028=CARTESIAN_POINT('Ctrl Pts',(-0.352910535259385,-1.96390792973863,
4.03444393336029));
#19029=CARTESIAN_POINT('Ctrl Pts',(1.45827126942817,-1.36195635287866,4.14555569806618));
#19030=CARTESIAN_POINT('Ctrl Pts',(1.93525541996257,0.486072691983231,4.25666746277205));
#19031=CARTESIAN_POINT('Ctrl Pts',(0.641640851567584,1.88938540800605,4.36777922747794));
#19032=CARTESIAN_POINT('Ctrl Pts',(-1.2390220506439,1.56406667389998,4.47889099218382));
#19033=CARTESIAN_POINT('Ctrl Pts',(-1.98608220824309,-0.192243763193254,
4.5900027568897));
#19034=CARTESIAN_POINT('Ctrl Pts',(-0.916041337559525,-1.77266705003184,
4.70111452159558));
#19035=CARTESIAN_POINT('Ctrl Pts',(0.992101626542076,-1.73124653501428,
4.81222628630146));
#19036=CARTESIAN_POINT('Ctrl Pts',(1.99255362081962,-0.105878565088393,
4.92333805100735));
#19037=CARTESIAN_POINT('Ctrl Pts',(1.16998377930773,1.61635953876083,5.03444981571323));
#19038=CARTESIAN_POINT('Ctrl Pts',(-0.72302449603639,1.85976229140111,5.14556158041912));
#19039=CARTESIAN_POINT('Ctrl Pts',(-1.95452513097788,0.401636296620756,
5.25667334512499));
#19040=CARTESIAN_POINT('Ctrl Pts',(-1.39779685446476,-1.42395370572007,
5.36778510983088));
#19041=CARTESIAN_POINT('Ctrl Pts',(0.43779998601491,-1.9467437876183,5.47889687453675));
#19042=CARTESIAN_POINT('Ctrl Pts',(1.8728460328454,-0.688424243942499,5.59000863924265));
#19043=CARTESIAN_POINT('Ctrl Pts',(1.59439279047996,1.19974656992392,5.70112040394852));
#19044=CARTESIAN_POINT('Ctrl Pts',(-0.142798044429764,1.99024845707447,
5.81223216865441));
#19045=CARTESIAN_POINT('Ctrl Pts',(-1.74934047402436,0.959837542695381,
5.92334393336029));
#19046=CARTESIAN_POINT('Ctrl Pts',(-1.75538099033144,-0.948745372113812,
6.03445569806617));
#19047=CARTESIAN_POINT('Ctrl Pts',(-0.155393020415026,-1.98930470556244,
6.14556746277206));
#19048=CARTESIAN_POINT('Ctrl Pts',(1.58676671675109,-1.20981469211756,6.25667922747794));
#19049=CARTESIAN_POINT('Ctrl Pts',(1.87716608811217,0.676555747555444,6.36779099218382));
#19050=CARTESIAN_POINT('Ctrl Pts',(0.45011367734252,1.94393360994604,6.4789027568897));
#19051=CARTESIAN_POINT('Ctrl Pts',(-1.38875553757466,1.43277292720395,6.59001452159559));
#19052=CARTESIAN_POINT('Ctrl Pts',(-1.95702824426536,-0.389256534908447,
6.70112628630146));
#19053=CARTESIAN_POINT('Ctrl Pts',(-0.734781901120652,-1.85514844727406,
6.81223805100735));
#19054=CARTESIAN_POINT('Ctrl Pts',(1.15972914243869,-1.62373289949622,6.92334981571322));
#19055=CARTESIAN_POINT('Ctrl Pts',(1.99318388502257,0.0932640175375246,
7.03446158041912));
#19056=CARTESIAN_POINT('Ctrl Pts',(1.00304017524133,1.72493206395685,7.14557334512499));
#19057=CARTESIAN_POINT('Ctrl Pts',(-0.904802416039021,1.7784298836705,7.25668510983089));
#19058=CARTESIAN_POINT('Ctrl Pts',(-1.98482551432077,0.20481136762979,7.36779687453676));
#19059=CARTESIAN_POINT('Ctrl Pts',(-1.24889751462265,-1.55619258434231,
7.47890863924264));
#19060=CARTESIAN_POINT('Ctrl Pts',(0.62966876606733,-1.89340903791239,7.59002040394853));
#19061=CARTESIAN_POINT('Ctrl Pts',(1.93213960395831,-0.498312631516818,
7.7011321686544));
#19062=CARTESIAN_POINT('Ctrl Pts',(1.46686353658972,1.35269840587584,7.8122439333603));
#19063=CARTESIAN_POINT('Ctrl Pts',(-0.340473492945126,1.96610267055844,
7.92335569806617));
#19064=CARTESIAN_POINT('Ctrl Pts',(-1.83630143665424,0.780684695965268,
8.03446746277206));
#19065=CARTESIAN_POINT('Ctrl Pts',(-1.65207296797424,-1.11899364274452,
8.14557922747793));
#19066=CARTESIAN_POINT('Ctrl Pts',(0.043680144826762,-1.99488833935353,
8.25669099218383));
#19067=CARTESIAN_POINT('Ctrl Pts',(1.69944200581072,-1.04561935177993,8.36780275688969));
#19068=CARTESIAN_POINT('Ctrl Pts',(1.80040735044495,0.860293905000138,8.47891452159559));
#19069=CARTESIAN_POINT('Ctrl Pts',(0.2540489856226,1.97913029706784,8.59002628630146));
#19070=CARTESIAN_POINT('Ctrl Pts',(-1.52455310456019,1.28718621537667,8.70113805100735));
#19071=CARTESIAN_POINT('Ctrl Pts',(-1.90867715688251,-0.58235090472488,
8.81224981571322));
#19072=CARTESIAN_POINT('Ctrl Pts',(-0.54582972530065,-1.91922982005443,
8.92336158041912));
#19073=CARTESIAN_POINT('Ctrl Pts',(1.31509067497552,-1.49989536946997,9.03447334512499));
#19074=CARTESIAN_POINT('Ctrl Pts',(1.97534232863193,0.291182401883861,9.14558510983087));
#19075=CARTESIAN_POINT('Ctrl Pts',(0.823290176095783,1.81696008473825,9.25669687453676));
#19076=CARTESIAN_POINT('Ctrl Pts',(-0.439363900704735,1.72408322084529,
9.33077138434068));
#19077=CARTESIAN_POINT('Ctrl Pts',(-0.911760019271175,1.42097259357916,
9.36780863924264));
#19078=CARTESIAN_POINT('Ctrl Pts',(0.903606778650207,-1.26612599672284,
-2.22044604925031E-15));
#19079=CARTESIAN_POINT('Ctrl Pts',(1.32452482391764,-0.965725878611127,
0.0370372549019586));
#19080=CARTESIAN_POINT('Ctrl Pts',(1.83597900638904,0.0826211852351528,
0.11111176470588));
#19081=CARTESIAN_POINT('Ctrl Pts',(0.924931235602245,1.59016045833715,0.222223529411763));
#19082=CARTESIAN_POINT('Ctrl Pts',(-0.83312512660499,1.63815347116992,0.333335294117645));
#19083=CARTESIAN_POINT('Ctrl Pts',(-1.82853441257778,0.189719885558947,
0.444447058823527));
#19084=CARTESIAN_POINT('Ctrl Pts',(-1.15119943064254,-1.43351224492194,
0.55555882352941));
#19085=CARTESIAN_POINT('Ctrl Pts',(0.579500018064921,-1.74455968620895,
0.666670588235291));
#19086=CARTESIAN_POINT('Ctrl Pts',(1.77994595636936,-0.459814902815864,
0.777782352941175));
#19087=CARTESIAN_POINT('Ctrl Pts',(1.35191942796293,1.24579875779621,0.888894117647056));
#19088=CARTESIAN_POINT('Ctrl Pts',(-0.31301785631821,1.81151698861828,1.00000588235294));
#19089=CARTESIAN_POINT('Ctrl Pts',(-1.69156114890735,0.719895542580366,
1.11111764705882));
#19090=CARTESIAN_POINT('Ctrl Pts',(-1.52247031399911,-1.03039633620486,
1.2222294117647));
#19091=CARTESIAN_POINT('Ctrl Pts',(0.0395573460867233,-1.83794734661457,
1.33334117647059));
#19092=CARTESIAN_POINT('Ctrl Pts',(1.56539206925502,-0.963935520329204,
1.44445294117647));
#19093=CARTESIAN_POINT('Ctrl Pts',(1.65902311109036,0.792001314055404,1.55556470588235));
#19094=CARTESIAN_POINT('Ctrl Pts',(0.234784819358076,1.82332048051019,1.66667647058823));
#19095=CARTESIAN_POINT('Ctrl Pts',(-1.40426199315134,1.18645316337148,1.77778823529412));
#19096=CARTESIAN_POINT('Ctrl Pts',(-1.75852526824674,-0.535921247894501,
1.88889999999999));
#19097=CARTESIAN_POINT('Ctrl Pts',(-0.503883253349445,-1.76797174153445,
2.00001176470588));
#19098=CARTESIAN_POINT('Ctrl Pts',(1.21177025569706,-1.38247440008765,2.11112352941176));
#19099=CARTESIAN_POINT('Ctrl Pts',(1.81875417317235,0.267872803846544,2.22223529411764));
#19100=CARTESIAN_POINT('Ctrl Pts',(0.761728374059259,1.67313849696631,2.33334705882353));
#19101=CARTESIAN_POINT('Ctrl Pts',(-0.992215910389441,1.54762080750275,
2.44445882352941));
#19102=CARTESIAN_POINT('Ctrl Pts',(-1.83836466671278,0.00615801197127806,
2.55557058823529));
#19103=CARTESIAN_POINT('Ctrl Pts',(-1.00256173219784,-1.54093884952435,
2.66668235294118));
#19104=CARTESIAN_POINT('Ctrl Pts',(0.750502303520728,-1.67820405842339,
2.77779411764705));
#19105=CARTESIAN_POINT('Ctrl Pts',(1.81691877690325,-0.280051291770722,
2.88890588235294));
#19106=CARTESIAN_POINT('Ctrl Pts',(1.221004776546,1.37432525375672,3.00001764705882));
#19107=CARTESIAN_POINT('Ctrl Pts',(-0.492027652059084,1.77130780998173,
3.11112941176471));
#19108=CARTESIAN_POINT('Ctrl Pts',(-1.75489545570189,0.547690156390568,
3.22224117647059));
#19109=CARTESIAN_POINT('Ctrl Pts',(-1.41217899707562,-1.17701871184488,
3.33335294117647));
#19110=CARTESIAN_POINT('Ctrl Pts',(0.2225644970039,-1.82485276462931,3.44446470588235));
#19111=CARTESIAN_POINT('Ctrl Pts',(1.65367987605646,-0.803097400934551,
3.55557647058823));
#19112=CARTESIAN_POINT('Ctrl Pts',(1.57181488059719,0.953425691385454,3.66668823529412));
#19113=CARTESIAN_POINT('Ctrl Pts',(0.05186921357973,1.83764309716413,3.7778));
#19114=CARTESIAN_POINT('Ctrl Pts',(-1.5155324957619,1.04056898961853,3.88891176470588));
#19115=CARTESIAN_POINT('Ctrl Pts',(-1.69634726272219,-0.708539718097244,
4.00002352941176));
#19116=CARTESIAN_POINT('Ctrl Pts',(-0.325144523748834,-1.80939315974833,
4.11113529411765));
#19117=CARTESIAN_POINT('Ctrl Pts',(1.34353857429153,-1.25480144535206,4.22224705882353));
#19118=CARTESIAN_POINT('Ctrl Pts',(1.7829949491126,0.447829855308947,4.33335882352941));
#19119=CARTESIAN_POINT('Ctrl Pts',(0.591158348240881,1.74073386109778,4.44447058823529));
#19120=CARTESIAN_POINT('Ctrl Pts',(-1.14153926936423,1.44101029294259,4.55558235294118));
#19121=CARTESIAN_POINT('Ctrl Pts',(-1.82982282818684,-0.177118562870956,
4.66669411764705));
#19122=CARTESIAN_POINT('Ctrl Pts',(-0.843969773291502,-1.63319857630279,
4.77780588235294));
#19123=CARTESIAN_POINT('Ctrl Pts',(0.914045851976043,-1.59503691128215,
4.88891764705882));
#19124=CARTESIAN_POINT('Ctrl Pts',(1.83578508816481,-0.0975483364234787,
5.0000294117647));
#19125=CARTESIAN_POINT('Ctrl Pts',(1.07793273566426,1.48918890180207,5.11114117647059));
#19126=CARTESIAN_POINT('Ctrl Pts',(-0.666138955726334,1.7134414082573,5.22225294117646));
#19127=CARTESIAN_POINT('Ctrl Pts',(-1.8007485732889,0.370036678811588,5.33336470588236));
#19128=CARTESIAN_POINT('Ctrl Pts',(-1.28782211675415,-1.31192102028485,
5.44447647058823));
#19129=CARTESIAN_POINT('Ctrl Pts',(0.403355110511087,-1.79357944420943,
5.55558823529412));
#19130=CARTESIAN_POINT('Ctrl Pts',(1.72549575760574,-0.634260954463495,
5.6667));
#19131=CARTESIAN_POINT('Ctrl Pts',(1.46895043569095,1.10535387335637,5.77781176470588));
#19132=CARTESIAN_POINT('Ctrl Pts',(-0.131563094636045,1.83366128824048,
5.88892352941177));
#19133=CARTESIAN_POINT('Ctrl Pts',(-1.61170726989826,0.884320215792288,
6.00003529411764));
#19134=CARTESIAN_POINT('Ctrl Pts',(-1.6172725353172,-0.874100746094603,
6.11114705882353));
#19135=CARTESIAN_POINT('Ctrl Pts',(-0.143167133221453,-1.83279178845155,
6.2222588235294));
#19136=CARTESIAN_POINT('Ctrl Pts',(1.46192436006299,-1.11462986392232,6.3333705882353));
#19137=CARTESIAN_POINT('Ctrl Pts',(1.72947592303562,0.623326238098233,6.44448235294117));
#19138=CARTESIAN_POINT('Ctrl Pts',(0.414699995127109,1.79099036343795,6.55559411764706));
#19139=CARTESIAN_POINT('Ctrl Pts',(-1.27949214532916,1.32004637014752,6.66670588235293));
#19140=CARTESIAN_POINT('Ctrl Pts',(-1.80305474864053,-0.358630922043501,
6.77781764705883));
#19141=CARTESIAN_POINT('Ctrl Pts',(-0.676971321141057,-1.70919056845102,
6.8889294117647));
#19142=CARTESIAN_POINT('Ctrl Pts',(1.06848490487467,-1.49598214718639,7.00004117647059));
#19143=CARTESIAN_POINT('Ctrl Pts',(1.83636576494725,0.0859262661083765,
7.11115294117646));
#19144=CARTESIAN_POINT('Ctrl Pts',(0.924123786330422,1.58921924510457,7.22226470588235));
#19145=CARTESIAN_POINT('Ctrl Pts',(-0.833615098607335,1.63850800634715,
7.33337647058823));
#19146=CARTESIAN_POINT('Ctrl Pts',(-1.82866500741913,0.188697383424353,
7.44448823529411));
#19147=CARTESIAN_POINT('Ctrl Pts',(-1.15063775952351,-1.4337557146759,7.5556));
#19148=CARTESIAN_POINT('Ctrl Pts',(0.580128192863429,-1.74444092308354,
7.66671176470588));
#19149=CARTESIAN_POINT('Ctrl Pts',(1.7801242767762,-0.459106790715335,7.77782352941176));
#19150=CARTESIAN_POINT('Ctrl Pts',(1.35145482596167,1.2462718876643,7.88893529411764));
#19151=CARTESIAN_POINT('Ctrl Pts',(-0.313685993055972,1.81141522451351,
8.00004705882353));
#19152=CARTESIAN_POINT('Ctrl Pts',(-1.69182638778816,0.719262612778256,
8.1111588235294));
#19153=CARTESIAN_POINT('Ctrl Pts',(-1.52209249852947,-1.03095436009227,
8.2222705882353));
#19154=CARTESIAN_POINT('Ctrl Pts',(0.0402435134914415,-1.83793611758998,
8.33338235294118));
#19155=CARTESIAN_POINT('Ctrl Pts',(1.56573467327064,-0.963352952631984,
8.44449411764705));
#19156=CARTESIAN_POINT('Ctrl Pts',(1.65875634765081,0.792608392434986,8.55560588235294));
#19157=CARTESIAN_POINT('Ctrl Pts',(0.234061123673802,1.82341787389281,8.66671764705882));
#19158=CARTESIAN_POINT('Ctrl Pts',(-1.40460554046006,1.18591401264663,8.7778294117647));
#19159=CARTESIAN_POINT('Ctrl Pts',(-1.75850778925809,-0.536533168193233,
8.88894117647058));
#19160=CARTESIAN_POINT('Ctrl Pts',(-0.502885372776985,-1.76823019847661,
9.00005294117646));
#19161=CARTESIAN_POINT('Ctrl Pts',(1.21162302759592,-1.38188780683742,9.11116470588235));
#19162=CARTESIAN_POINT('Ctrl Pts',(1.81992793219366,0.268272986849182,9.22227647058824));
#19163=CARTESIAN_POINT('Ctrl Pts',(0.758516013178858,1.6740067592164,9.33338823529411));
#19164=CARTESIAN_POINT('Ctrl Pts',(-0.404795980777633,1.58843718658925,
9.40746274509804));
#19165=CARTESIAN_POINT('Ctrl Pts',(-0.840025297123196,1.30917445368946,
9.4445));
#19166=CARTESIAN_POINT('',(0.903606778650208,-1.26612599672284,0.));
#19167=CARTESIAN_POINT('Ctrl Pts',(0.903606778650207,-1.26612599672284,
-2.22044604925031E-15));
#19168=CARTESIAN_POINT('Ctrl Pts',(1.32452482391764,-0.965725878611127,
0.0370372549019586));
#19169=CARTESIAN_POINT('Ctrl Pts',(1.83597900638904,0.0826211852351528,
0.11111176470588));
#19170=CARTESIAN_POINT('Ctrl Pts',(0.924931235602245,1.59016045833715,0.222223529411763));
#19171=CARTESIAN_POINT('Ctrl Pts',(-0.83312512660499,1.63815347116992,0.333335294117645));
#19172=CARTESIAN_POINT('Ctrl Pts',(-1.53106292762084,0.622574687744289,
0.411242042445823));
#19173=CARTESIAN_POINT('Ctrl Pts',(-1.55772933110463,0.0543333176694591,
0.452111535872041));
#19174=CARTESIAN_POINT('Ctrl Pts',(-1.55735939632673,0.00101326450419686,
0.455943774396298));
#19175=CARTESIAN_POINT('Ctrl Pts',(0.863568020353686,1.756414520678,-8.67361737988404E-17));
#19176=CARTESIAN_POINT('Ctrl Pts',(0.902604744553569,1.73244180767701,-8.9279167384606E-17));
#19177=CARTESIAN_POINT('Ctrl Pts',(0.940679665251258,1.70703474391515,8.97961926050354E-17));
#19178=CARTESIAN_POINT('Ctrl Pts',(0.977702286264215,1.68018861076749,5.72458747072346E-17));
#19179=CARTESIAN_POINT('Ctrl Pts',(1.03586153234927,1.63801572236987,1.46490398407746E-17));
#19180=CARTESIAN_POINT('Ctrl Pts',(1.09142617933376,1.59229270785348,-2.67869138917656E-16));
#19181=CARTESIAN_POINT('Ctrl Pts',(1.14423485590453,1.54336034436958,-3.57353036051222E-16));
#19182=CARTESIAN_POINT('Ctrl Pts',(1.16947315095921,1.51997461483563,-4.00119133313148E-16));
#19183=CARTESIAN_POINT('Ctrl Pts',(1.19408133665882,1.49585539554391,8.18581218658372E-17));
#19184=CARTESIAN_POINT('Ctrl Pts',(1.21803815377257,1.47103794919798,5.55111512312578E-17));
#19185=CARTESIAN_POINT('Ctrl Pts',(1.23019217561359,1.45844730397601,4.21445318253017E-17));
#19186=CARTESIAN_POINT('Ctrl Pts',(1.24217850624866,1.44567693083781,1.93655380221213E-16));
#19187=CARTESIAN_POINT('Ctrl Pts',(1.25399412029808,1.43273135759888,2.04697370165263E-16));
#19188=CARTESIAN_POINT('Ctrl Pts',(1.26387705342325,1.42190329279817,2.13933220941147E-16));
#19189=CARTESIAN_POINT('Ctrl Pts',(1.27363384828941,1.41095997328553,2.33605914868334E-16));
#19190=CARTESIAN_POINT('Ctrl Pts',(1.28326192166555,1.39990597410978,2.08166817117217E-16));
#19191=CARTESIAN_POINT('Ctrl Pts',(1.33014969679031,1.34607407988414,8.42809005758918E-17));
#19192=CARTESIAN_POINT('Ctrl Pts',(1.37399942421539,1.28960720074626,-1.13965484205857E-16));
#19193=CARTESIAN_POINT('Ctrl Pts',(1.4146477049008,1.230839634391,-1.87350135405495E-16));
#19194=CARTESIAN_POINT('Ctrl Pts',(1.44368896684187,1.18885300520561,-2.39779976028666E-16));
#19195=CARTESIAN_POINT('Ctrl Pts',(1.47109515917518,1.14569133662427,-8.7819322856054E-17));
#19196=CARTESIAN_POINT('Ctrl Pts',(1.49679111505729,1.10147172806437,-6.24500451351651E-17));
#19197=CARTESIAN_POINT('Ctrl Pts',(1.51163881269315,1.07592064989137,-4.77911094423959E-17));
#19198=CARTESIAN_POINT('Ctrl Pts',(1.52591525031524,1.05001629664473,1.5220027212751E-16));
#19199=CARTESIAN_POINT('Ctrl Pts',(1.53960379146143,1.02378110502453,1.66533453693773E-16));
#19200=CARTESIAN_POINT('Ctrl Pts',(1.54537176342799,1.01272632218197,1.72573059272106E-16));
#19201=CARTESIAN_POINT('Ctrl Pts',(1.55103093390346,1.00162120437101,-1.75133660485687E-16));
#19202=CARTESIAN_POINT('Ctrl Pts',(1.55657976538519,0.990469147617543,-1.87350135405495E-16));
#19203=CARTESIAN_POINT('Ctrl Pts',(1.58759368815465,0.928137280446804,-2.55631324143141E-16));
#19204=CARTESIAN_POINT('Ctrl Pts',(1.61517308010414,0.864324080823349,1.42069026423598E-16));
#19205=CARTESIAN_POINT('Ctrl Pts',(1.63916386047712,0.799337824232817,2.77555756156289E-17));
#19206=CARTESIAN_POINT('Ctrl Pts',(1.66256346318323,0.735952950463245,-8.37409781139008E-17));
#19207=CARTESIAN_POINT('Ctrl Pts',(1.68254922594952,0.671451147944667,-8.96615244715113E-17));
#19208=CARTESIAN_POINT('Ctrl Pts',(1.69892983273053,0.606113461272593,-9.71445146547012E-17));
#19209=CARTESIAN_POINT('Ctrl Pts',(1.70969890177119,0.563158638650024,-1.02064041689972E-16));
#19210=CARTESIAN_POINT('Ctrl Pts',(1.71890879491296,0.519842467826019,-3.45159500757614E-16));
#19211=CARTESIAN_POINT('Ctrl Pts',(1.72649301018808,0.476246530743055,-3.05311331771918E-16));
#19212=CARTESIAN_POINT('Ctrl Pts',(1.73286946004292,0.43959312671897,-2.71808874084789E-16));
#19213=CARTESIAN_POINT('Ctrl Pts',(1.7380966173026,0.40274196097511,-2.63721634519194E-16));
#19214=CARTESIAN_POINT('Ctrl Pts',(1.74212938372161,0.365743253928757,-2.91433543964104E-16));
#19215=CARTESIAN_POINT('Ctrl Pts',(1.74338441815136,0.3542289120664,-3.00057748010143E-16));
#19216=CARTESIAN_POINT('Ctrl Pts',(1.74452367514155,0.342699905808242,-2.95319042101862E-16));
#19217=CARTESIAN_POINT('Ctrl Pts',(1.74554463432397,0.331172964307001,-2.77555756156289E-16));
#19218=CARTESIAN_POINT('Ctrl Pts',(1.75129363197339,0.266265022112653,-1.77531101983038E-16));
#19219=CARTESIAN_POINT('Ctrl Pts',(1.75330947147495,0.201304509751005,-1.61672294252907E-16));
#19220=CARTESIAN_POINT('Ctrl Pts',(1.75142501653378,0.136551819838445,-1.94289029309402E-16));
#19221=CARTESIAN_POINT('Ctrl Pts',(1.75088238549665,0.117906205917838,-2.03681056884401E-16));
#19222=CARTESIAN_POINT('Ctrl Pts',(1.75001603328345,0.0992778655205717,
5.11497906607206E-18));
#19223=CARTESIAN_POINT('Ctrl Pts',(1.74882116957219,0.0806731627252344,
-1.38777878078145E-17));
#19224=CARTESIAN_POINT('Ctrl Pts',(1.74442035560002,0.0121500037758971,
-8.61363537235156E-17));
#19225=CARTESIAN_POINT('Ctrl Pts',(1.73556731065817,-0.0560546348769042,
-8.94984743174132E-17));
#19226=CARTESIAN_POINT('Ctrl Pts',(1.72245500570668,-0.123603583729898,
-1.11022302462516E-16));
#19227=CARTESIAN_POINT('Ctrl Pts',(1.71065372503254,-0.184398700042928,
-1.30394086299314E-16));
#19228=CARTESIAN_POINT('Ctrl Pts',(1.69540112401956,-0.244662986427059,
-2.83658263324553E-17));
#19229=CARTESIAN_POINT('Ctrl Pts',(1.67680526621061,-0.304125446889571,
0.));
#19230=CARTESIAN_POINT('Ctrl Pts',(1.67349606673433,-0.31470700462369,5.04780035468084E-18));
#19231=CARTESIAN_POINT('Ctrl Pts',(1.67008251071857,-0.325257870756687,
-2.59895781250022E-16));
#19232=CARTESIAN_POINT('Ctrl Pts',(1.66656792507904,-0.33576950432459,-2.4980018054066E-16));
#19233=CARTESIAN_POINT('Ctrl Pts',(1.64601555867501,-0.397238754685905,
-1.90763780199754E-16));
#19234=CARTESIAN_POINT('Ctrl Pts',(1.62198854159901,-0.457444427764366,
-5.62956498032537E-16));
#19235=CARTESIAN_POINT('Ctrl Pts',(1.59467348808245,-0.516112566668481,
-4.9960036108132E-16));
#19236=CARTESIAN_POINT('Ctrl Pts',(1.5674666304738,-0.574548318967516,-4.36495180063804E-16));
#19237=CARTESIAN_POINT('Ctrl Pts',(1.53699697643864,-0.631459529320744,
-5.34526979994394E-16));
#19238=CARTESIAN_POINT('Ctrl Pts',(1.50340933089056,-0.686542989409802,
-5.27355936696949E-16));
#19239=CARTESIAN_POINT('Ctrl Pts',(1.47050931920745,-0.740498735664251,
-5.20331704887418E-16));
#19240=CARTESIAN_POINT('Ctrl Pts',(1.43461693006704,-0.792701424833635,
-2.68404534867939E-16));
#19241=CARTESIAN_POINT('Ctrl Pts',(1.39584139349689,-0.842824299455657,
-2.22044604925031E-16));
#19242=CARTESIAN_POINT('Ctrl Pts',(1.38890909242928,-0.851785280733763,
-2.13756363929169E-16));
#19243=CARTESIAN_POINT('Ctrl Pts',(1.38188458496569,-0.860679662653787,
-1.66156715466689E-16));
#19244=CARTESIAN_POINT('Ctrl Pts',(1.37476842993966,-0.869505410466454,
-1.66533453693773E-16));
#19245=CARTESIAN_POINT('Ctrl Pts',(1.36798353599758,-0.877920314673783,
-1.6689265454105E-16));
#19246=CARTESIAN_POINT('Ctrl Pts',(1.36111848029899,-0.886268835999708,
-1.80781753969063E-16));
#19247=CARTESIAN_POINT('Ctrl Pts',(1.35417907408573,-0.894543489490856,
-1.66533453693773E-16));
#19248=CARTESIAN_POINT('Ctrl Pts',(1.31430606770251,-0.942088668621772,
-8.46644075005493E-17));
#19249=CARTESIAN_POINT('Ctrl Pts',(1.27193077516495,-0.987260711017392,
3.92232772703659E-16));
#19250=CARTESIAN_POINT('Ctrl Pts',(1.22719194772877,-1.02979240857164,3.33066907387547E-16));
#19251=CARTESIAN_POINT('Ctrl Pts',(1.18325774198238,-1.07155917936502,2.74965132063436E-16));
#19252=CARTESIAN_POINT('Ctrl Pts',(1.13704354519755,-1.11078025986631,2.70799735769765E-17));
#19253=CARTESIAN_POINT('Ctrl Pts',(1.08865738848829,-1.14715869099291,2.77555756156289E-17));
#19254=CARTESIAN_POINT('Ctrl Pts',(1.04181551274958,-1.18237607683823,2.84096153016807E-17));
#19255=CARTESIAN_POINT('Ctrl Pts',(0.992937497203575,-1.21492966574416,
-2.26622882727394E-16));
#19256=CARTESIAN_POINT('Ctrl Pts',(0.942108816666581,-1.24450267784172,
-2.22044604925031E-16));
#19257=CARTESIAN_POINT('Ctrl Pts',(0.929396434173388,-1.25189896350738,
-2.20899565983063E-16));
#19258=CARTESIAN_POINT('Ctrl Pts',(0.916561996392962,-1.25910856034592,
-5.43661122892894E-17));
#19259=CARTESIAN_POINT('Ctrl Pts',(0.903606778650232,-1.26612599672282,
-5.55111512312578E-17));
#19260=CARTESIAN_POINT('Ctrl Pts',(1.57638112755711,1.1485113017068,9.04599999999999));
#19261=CARTESIAN_POINT('Ctrl Pts',(1.76277867682249,0.89337775104729,9.02806746277205));
#19262=CARTESIAN_POINT('Ctrl Pts',(1.89066037358035,0.595600609460199,9.01013492554411));
#19263=CARTESIAN_POINT('Ctrl Pts',(1.93659149294971,0.285826861476621,8.99220238831616));
#19264=CARTESIAN_POINT('Ctrl Pts',(2.03145607091723,-0.35396934360954,8.95516513341421));
#19265=CARTESIAN_POINT('Ctrl Pts',(1.77674102032598,-1.04493991917229,8.91812787851224));
#19266=CARTESIAN_POINT('Ctrl Pts',(1.29042609501658,-1.47131163503284,8.88109062361028));
#19267=CARTESIAN_POINT('Ctrl Pts',(0.804111169707157,-1.8976833508934,8.84405336870832));
#19268=CARTESIAN_POINT('Ctrl Pts',(0.086196369679569,-2.05945620705174,
8.80701611380637));
#19269=CARTESIAN_POINT('Ctrl Pts',(-0.535643940631454,-1.88246885422725,
8.7699788589044));
#19270=CARTESIAN_POINT('Ctrl Pts',(-1.15748425094246,-1.70548150140276,
8.73294160400244));
#19271=CARTESIAN_POINT('Ctrl Pts',(-1.68325007153691,-1.18973393959546,
8.69590434910048));
#19272=CARTESIAN_POINT('Ctrl Pts',(-1.87203837193898,-0.571240658920998,
8.65886709419851));
#19273=CARTESIAN_POINT('Ctrl Pts',(-1.92810375324022,-0.387563696209775,
8.64786796017375));
#19274=CARTESIAN_POINT('Ctrl Pts',(-1.95444971403581,-0.194825169918805,
8.63686882614899));
#19275=CARTESIAN_POINT('Ctrl Pts',(-1.95285709583883,-0.00166548583676096,
8.62586969212423));
#19276=CARTESIAN_POINT('Origin',(0.,0.,-1.2940562256037));
#19277=CARTESIAN_POINT('',(-0.903606778650184,-1.26612599672285,-1.38777878078145E-16));
#19278=CARTESIAN_POINT('Ctrl Pts',(-0.905550660636142,-1.26792405592273,
1.1310939164455E-15));
#19279=CARTESIAN_POINT('Ctrl Pts',(-0.51353745480643,-1.54485763355445,
0.0345106401883014));
#19280=CARTESIAN_POINT('Ctrl Pts',(0.588170214887261,-1.72164661131011,
0.106088614025153));
#19281=CARTESIAN_POINT('Ctrl Pts',(1.77543639638611,-0.478750755853424,
0.214733921510558));
#19282=CARTESIAN_POINT('Ctrl Pts',(1.36425885975684,1.23323526260274,0.325935922456214));
#19283=CARTESIAN_POINT('Ctrl Pts',(-0.297175317740204,1.81462004446968,
0.43713792340187));
#19284=CARTESIAN_POINT('Ctrl Pts',(-1.41354004632119,0.945824564565656,
0.526511357784366));
#19285=CARTESIAN_POINT('Ctrl Pts',(-1.55416372641,0.214215408672241,0.578817458518311));
#19286=CARTESIAN_POINT('Ctrl Pts',(-1.55326674879324,0.000737490386717929,
0.594056225603704));
#19287=CARTESIAN_POINT('Origin',(0.,0.,0.));
#19288=CARTESIAN_POINT('Ctrl Pts',(-0.685825729128738,1.39614588036675,
-0.230074082272066));
#19289=CARTESIAN_POINT('Ctrl Pts',(-1.1503452556824,1.16796095537201,-0.193006748623514));
#19290=CARTESIAN_POINT('Ctrl Pts',(-1.82566639114231,0.215444531932564,
-0.11887208132641));
#19291=CARTESIAN_POINT('Ctrl Pts',(-1.16908877997113,-1.42098933913104,
-0.00767008038075383));
#19292=CARTESIAN_POINT('Ctrl Pts',(0.560230897929427,-1.75089503242436,
0.103531920564902));
#19293=CARTESIAN_POINT('Ctrl Pts',(1.77543639638611,-0.478750755853424,
0.214733921510558));
#19294=CARTESIAN_POINT('Ctrl Pts',(1.36425885975684,1.23323526260274,0.325935922456214));
#19295=CARTESIAN_POINT('Ctrl Pts',(-0.297175317740204,1.81462004446968,
0.43713792340187));
#19296=CARTESIAN_POINT('Ctrl Pts',(-1.68620095450898,0.733629966765004,
0.548339924347525));
#19297=CARTESIAN_POINT('Ctrl Pts',(-1.53025640912295,-1.01973871733877,
0.659541925293182));
#19298=CARTESIAN_POINT('Ctrl Pts',(0.0278603330084876,-1.83865390028585,
0.770743926238836));
#19299=CARTESIAN_POINT('Ctrl Pts',(1.5604328654528,-0.972896783194139,0.881945927184494));
#19300=CARTESIAN_POINT('Ctrl Pts',(1.66322297628929,0.784329206349798,0.993147928130148));
#19301=CARTESIAN_POINT('Ctrl Pts',(0.242033178606095,1.82287837028977,1.10434992907581));
#19302=CARTESIAN_POINT('Ctrl Pts',(-1.40092403541303,1.19117010090687,1.21555193002146));
#19303=CARTESIAN_POINT('Ctrl Pts',(-1.76024597462735,-0.531985223933843,
1.32675393096712));
#19304=CARTESIAN_POINT('Ctrl Pts',(-0.506691785521986,-1.76769208329225,
1.43795593191277));
#19305=CARTESIAN_POINT('Ctrl Pts',(1.21113283005724,-1.38370173748454,1.54915793285843));
#19306=CARTESIAN_POINT('Ctrl Pts',(1.81922269924897,0.268145221691032,1.66035993380409));
#19307=CARTESIAN_POINT('Ctrl Pts',(0.760397896971566,1.67429621989364,1.77156193474974));
#19308=CARTESIAN_POINT('Ctrl Pts',(-0.99516307107971,1.54632579451077,1.8827639356954));
#19309=CARTESIAN_POINT('Ctrl Pts',(-1.83887757709731,0.00149027413755925,
1.99396593664105));
#19310=CARTESIAN_POINT('Ctrl Pts',(-0.997668151382599,-1.54471071329041,
2.10516793758671));
#19311=CARTESIAN_POINT('Ctrl Pts',(0.757683106401647,-1.67552656471375,
2.21636993853236));
#19312=CARTESIAN_POINT('Ctrl Pts',(1.81878565659978,-0.271093501731151,
2.32757193947802));
#19313=CARTESIAN_POINT('Ctrl Pts',(1.2133740808,1.38173669240563,2.43877394042368));
#19314=CARTESIAN_POINT('Ctrl Pts',(-0.50382603046139,1.76851131819754,2.54997594136933));
#19315=CARTESIAN_POINT('Ctrl Pts',(-1.75938120199744,0.534837111883675,
2.66117794231499));
#19316=CARTESIAN_POINT('Ctrl Pts',(-1.40285327152777,-1.18889681987293,
2.77237994326064));
#19317=CARTESIAN_POINT('Ctrl Pts',(0.239078896742882,-1.82327020255007,
2.88358194420631));
#19318=CARTESIAN_POINT('Ctrl Pts',(1.66194822130476,-0.787020368122459,
2.99478394515195));
#19319=CARTESIAN_POINT('Ctrl Pts',(1.56201018579718,0.970359278599158,3.10598594609762));
#19320=CARTESIAN_POINT('Ctrl Pts',(0.0308358597469676,1.83861961806662,
3.21718794704326));
#19321=CARTESIAN_POINT('Ctrl Pts',(-1.52859270045602,1.02219240178121,3.32838994798893));
#19322=CARTESIAN_POINT('Ctrl Pts',(-1.68740469215855,-0.730847696189792,
3.43959194893457));
#19323=CARTESIAN_POINT('Ctrl Pts',(-0.300084107876245,-1.81422779119842,
3.55079394988024));
#19324=CARTESIAN_POINT('Ctrl Pts',(1.36219708122283,-1.23527003608861,3.66199595082589));
#19325=CARTESIAN_POINT('Ctrl Pts',(1.77632642388981,0.475539047756765,3.77319795177155));
#19326=CARTESIAN_POINT('Ctrl Pts',(0.562846122986205,1.75062194433623,3.8843999527172));
#19327=CARTESIAN_POINT('Ctrl Pts',(-1.16635795779188,1.42164765833408,3.99560195366286));
#19328=CARTESIAN_POINT('Ctrl Pts',(-1.82685336294205,-0.209951757455398,
4.10680395460851));
#19329=CARTESIAN_POINT('Ctrl Pts',(-0.813442378520323,-1.64917689984389,
4.21800595555418));
#19330=CARTESIAN_POINT('Ctrl Pts',(0.945308337362415,-1.57729676898942,
4.32920795649982));
#19331=CARTESIAN_POINT('Ctrl Pts',(1.83789338383513,-0.0601735806349488,
4.44040995744549));
#19332=CARTESIAN_POINT('Ctrl Pts',(1.04645630737228,1.51208536363268,4.55161195839114));
#19333=CARTESIAN_POINT('Ctrl Pts',(-0.703826144888774,1.69885305660096,
4.66281395933679));
#19334=CARTESIAN_POINT('Ctrl Pts',(-1.80920785964355,0.328998283818298,
4.77401596028245));
#19335=CARTESIAN_POINT('Ctrl Pts',(-1.25685137944873,-1.34231053043966,
4.88521796122811));
#19336=CARTESIAN_POINT('Ctrl Pts',(0.447130949584586,-1.78368911643119,
4.99641996217376));
#19337=CARTESIAN_POINT('Ctrl Pts',(1.74141681985029,-0.590711782254083,
5.10762196311942));
#19338=CARTESIAN_POINT('Ctrl Pts',(1.44007996484097,1.14352203521175,5.21882396406507));
#19339=CARTESIAN_POINT('Ctrl Pts',(-0.18077114541208,1.82997124106871,5.33002596501073));
#19340=CARTESIAN_POINT('Ctrl Pts',(-1.63598554858516,0.839657212778587,
5.44122796595639));
#19341=CARTESIAN_POINT('Ctrl Pts',(-1.5921816295577,-0.920016634985102,
5.55242996690203));
#19342=CARTESIAN_POINT('Ctrl Pts',(-0.089495975882287,-1.83669905549533,
5.66363196784771));
#19343=CARTESIAN_POINT('Ctrl Pts',(1.49519291292304,-1.07045369039924,5.77483396879335));
#19344=CARTESIAN_POINT('Ctrl Pts',(1.70986873918469,0.676625335695913,5.88603596973901));
#19345=CARTESIAN_POINT('Ctrl Pts',(0.357828666998206,1.80372713991337,5.99723797068467));
#19346=CARTESIAN_POINT('Ctrl Pts',(-1.32208210581628,1.27811261459153,6.10843997163031));
#19347=CARTESIAN_POINT('Ctrl Pts',(-1.79059752017374,-0.418608971338806,
6.21964197257599));
#19348=CARTESIAN_POINT('Ctrl Pts',(-0.618426992791356,-1.73176817298442,
6.33084397352162));
#19349=CARTESIAN_POINT('Ctrl Pts',(1.12039486833334,-1.45814549642773,6.4420459744673));
#19350=CARTESIAN_POINT('Ctrl Pts',(1.83262304280178,0.151544492417154,6.55324797541294));
#19351=CARTESIAN_POINT('Ctrl Pts',(0.865658194202354,1.62237752769619,6.6644499763586));
#19352=CARTESIAN_POINT('Ctrl Pts',(-0.894490612933678,1.60666097558597,
6.77565197730426));
#19353=CARTESIAN_POINT('Ctrl Pts',(-1.83503693743053,0.11879557904028,6.8868539782499));
#19354=CARTESIAN_POINT('Ctrl Pts',(-1.09417843856274,-1.47791965389608,
6.99805597919557));
#19355=CARTESIAN_POINT('Ctrl Pts',(0.649252195647424,-1.72044892818251,
7.10925798014122));
#19356=CARTESIAN_POINT('Ctrl Pts',(1.79778702933405,-0.386567926277561,
7.22045998108688));
#19357=CARTESIAN_POINT('Ctrl Pts',(1.29904832373936,1.30151698160267,7.33166198203254));
#19358=CARTESIAN_POINT('Ctrl Pts',(-0.389980372076409,1.79704983321667,
7.44286398297819));
#19359=CARTESIAN_POINT('Ctrl Pts',(-1.72167847110372,0.645984776536109,
7.55406598392385));
#19360=CARTESIAN_POINT('Ctrl Pts',(-1.47583963303223,-1.09698250119657,
7.6652679848695));
#19361=CARTESIAN_POINT('Ctrl Pts',(0.122279206149944,-1.83480779990519,
7.77646998581516));
#19362=CARTESIAN_POINT('Ctrl Pts',(1.6083563717128,-0.891439258304551,7.88767198676082));
#19363=CARTESIAN_POINT('Ctrl Pts',(1.6207309884821,0.868737834600438,7.99887398770647));
#19364=CARTESIAN_POINT('Ctrl Pts',(0.148065176955119,1.83290543012718,8.11007598865213));
#19365=CARTESIAN_POINT('Ctrl Pts',(-1.46027046044108,1.11762836182387,8.22127798959778));
#19366=CARTESIAN_POINT('Ctrl Pts',(-1.73059002514951,-0.621721033251858,
8.33247999054344));
#19367=CARTESIAN_POINT('Ctrl Pts',(-0.415210463238687,-1.79137506804378,
8.4436819914891));
#19368=CARTESIAN_POINT('Ctrl Pts',(1.28062367350908,-1.31967978545922,8.55488399243474));
#19369=CARTESIAN_POINT('Ctrl Pts',(1.80303816946195,0.361303122856545,8.66608599338042));
#19370=CARTESIAN_POINT('Ctrl Pts',(0.673390003682997,1.71105376251155,8.77728799432605));
#19371=CARTESIAN_POINT('Ctrl Pts',(-1.07331353684551,1.49334172277348,8.88848999527173));
#19372=CARTESIAN_POINT('Ctrl Pts',(-1.83648185490594,-0.0933331690448563,
8.99969199621736));
#19373=CARTESIAN_POINT('Ctrl Pts',(-0.917075781704608,-1.59325581253419,
9.11089399716304));
#19374=CARTESIAN_POINT('Ctrl Pts',(0.84291969341562,-1.63568507599433,9.22209599810868));
#19375=CARTESIAN_POINT('Ctrl Pts',(1.83002015964776,-0.174643446395858,
9.33329799905435));
#19376=CARTESIAN_POINT('Ctrl Pts',(1.37089695500413,0.898926325849287,9.40743266635145));
#19377=CARTESIAN_POINT('Ctrl Pts',(0.964986447796868,1.2199923793075,9.4445));
#19378=CARTESIAN_POINT('Ctrl Pts',(-0.744392439309333,1.51537102412035,
-0.153382721514711));
#19379=CARTESIAN_POINT('Ctrl Pts',(-1.24858003215071,1.26770004049271,-0.116315387866159));
#19380=CARTESIAN_POINT('Ctrl Pts',(-1.98157082848726,0.233842613144434,
-0.0421807205690546));
#19381=CARTESIAN_POINT('Ctrl Pts',(-1.26892417669641,-1.54233601257873,
0.0690212803766013));
#19382=CARTESIAN_POINT('Ctrl Pts',(0.60807232358566,-1.90041430177422,0.180223281322257));
#19383=CARTESIAN_POINT('Ctrl Pts',(1.92705139777042,-0.519634110874885,
0.291425282267913));
#19384=CARTESIAN_POINT('Ctrl Pts',(1.48076098246403,1.33854850639298,0.402627283213569));
#19385=CARTESIAN_POINT('Ctrl Pts',(-0.32255287353564,1.96958116902152,0.513829284159225));
#19386=CARTESIAN_POINT('Ctrl Pts',(-1.83019561439793,0.796278963176857,
0.62503128510488));
#19387=CARTESIAN_POINT('Ctrl Pts',(-1.6609340431175,-1.10682023000553,0.736233286050537));
#19388=CARTESIAN_POINT('Ctrl Pts',(0.0302394914149615,-1.99566741775375,
0.847435286996192));
#19389=CARTESIAN_POINT('Ctrl Pts',(1.69368744530556,-1.05597818640917,0.958637287941849));
#19390=CARTESIAN_POINT('Ctrl Pts',(1.80525541088723,0.85130771031001,1.0698392888875));
#19391=CARTESIAN_POINT('Ctrl Pts',(0.262701821416467,1.97854472206529,1.18104128983316));
#19392=CARTESIAN_POINT('Ctrl Pts',(-1.52055721405056,1.29289115206115,1.29224329077882));
#19393=CARTESIAN_POINT('Ctrl Pts',(-1.91056377616791,-0.577414584640491,
1.40344529172447));
#19394=CARTESIAN_POINT('Ctrl Pts',(-0.549961190114417,-1.91864575203584,
1.51464729267013));
#19395=CARTESIAN_POINT('Ctrl Pts',(1.31455861657342,-1.50186420236992,1.62584929361578));
#19396=CARTESIAN_POINT('Ctrl Pts',(1.97457687168029,0.291043726104147,1.73705129456144));
#19397=CARTESIAN_POINT('Ctrl Pts',(0.825332765061831,1.81727426417256,1.8482532955071));
#19398=CARTESIAN_POINT('Ctrl Pts',(-1.08014592414415,1.67837568824538,1.95945529645275));
#19399=CARTESIAN_POINT('Ctrl Pts',(-1.99591019564939,0.00161753744922554,
2.07065729739841));
#19400=CARTESIAN_POINT('Ctrl Pts',(-1.08286492805163,-1.67662268569932,
2.18185929834406));
#19401=CARTESIAN_POINT('Ctrl Pts',(0.822386142488863,-1.81860967540451,
2.29306129928972));
#19402=CARTESIAN_POINT('Ctrl Pts',(1.97410250737766,-0.294243777192403,
2.40426330023538));
#19403=CARTESIAN_POINT('Ctrl Pts',(1.31699126095619,1.49973135048419,2.51546530118103));
#19404=CARTESIAN_POINT('Ctrl Pts',(-0.546850711301162,1.91953494624891,
2.62666730212668));
#19405=CARTESIAN_POINT('Ctrl Pts',(-1.90962515549492,0.58051001214848,2.73786930307235));
#19406=CARTESIAN_POINT('Ctrl Pts',(-1.52265119903315,-1.29042374213144,
2.849071304018));
#19407=CARTESIAN_POINT('Ctrl Pts',(0.259495255973991,-1.97897001519685,
2.96027330496365));
#19408=CARTESIAN_POINT('Ctrl Pts',(1.80387179704459,-0.854228686283152,
3.07147530590931));
#19409=CARTESIAN_POINT('Ctrl Pts',(1.69539946235139,1.05322398930777,3.18267730685497));
#19410=CARTESIAN_POINT('Ctrl Pts',(0.0334691159580969,1.99563020797331,
3.29387930780062));
#19411=CARTESIAN_POINT('Ctrl Pts',(-1.65912826053996,1.10948344905644,3.40508130874628));
#19412=CARTESIAN_POINT('Ctrl Pts',(-1.83150214631588,-0.793259098082338,
3.51628330969193));
#19413=CARTESIAN_POINT('Ctrl Pts',(-0.325710062443639,-1.96915541892639,
3.62748531063759));
#19414=CARTESIAN_POINT('Ctrl Pts',(1.47852313648206,-1.34075704120622,3.73868731158324));
#19415=CARTESIAN_POINT('Ctrl Pts',(1.92801742998006,0.516148136052275,3.84988931252891));
#19416=CARTESIAN_POINT('Ctrl Pts',(0.610910878158188,1.90011789308111,3.96109131347456));
#19417=CARTESIAN_POINT('Ctrl Pts',(-1.26596015348029,1.54305054954723,4.07229331442022));
#19418=CARTESIAN_POINT('Ctrl Pts',(-1.98285916282043,-0.227880778208832,
4.18349531536587));
#19419=CARTESIAN_POINT('Ctrl Pts',(-0.882907028223612,-1.79000985700403,
4.29469731631152));
#19420=CARTESIAN_POINT('Ctrl Pts',(1.02603380022298,-1.71199145718021,4.40589931725719));
#19421=CARTESIAN_POINT('Ctrl Pts',(1.99484195631093,-0.0653121581305224,
4.51710131820284));
#19422=CARTESIAN_POINT('Ctrl Pts',(1.13581939287274,1.64121126471649,4.62830331914849));
#19423=CARTESIAN_POINT('Ctrl Pts',(-0.763930016899512,1.84392815422348,
4.73950532009415));
#19424=CARTESIAN_POINT('Ctrl Pts',(-1.96370680576333,0.357093390665327,
4.8507073210398));
#19425=CARTESIAN_POINT('Ctrl Pts',(-1.36418134295679,-1.45693835565774,
4.96190932198546));
#19426=CARTESIAN_POINT('Ctrl Pts',(0.485314102570633,-1.93600886632894,
5.07311132293112));
#19427=CARTESIAN_POINT('Ctrl Pts',(1.89012668864067,-0.64115615067331,5.18431332387677));
#19428=CARTESIAN_POINT('Ctrl Pts',(1.56305689958632,1.24117413657934,5.29551532482243));
#19429=CARTESIAN_POINT('Ctrl Pts',(-0.196208261333358,1.98624329497761,
5.40671732576808));
#19430=CARTESIAN_POINT('Ctrl Pts',(-1.77569201834004,0.911360502030131,
5.51791932671374));
#19431=CARTESIAN_POINT('Ctrl Pts',(-1.72814742391724,-0.998582289981674,
5.6291213276594));
#19432=CARTESIAN_POINT('Ctrl Pts',(-0.0971385659153217,-1.9935456372193,
5.74032332860505));
#19433=CARTESIAN_POINT('Ctrl Pts',(1.62287626785709,-1.16186605418883,5.8515253295507));
#19434=CARTESIAN_POINT('Ctrl Pts',(1.85588453101264,0.734406369934583,5.96272733049637));
#19435=CARTESIAN_POINT('Ctrl Pts',(0.388385770565944,1.95775805500079,6.07392933144201));
#19436=CARTESIAN_POINT('Ctrl Pts',(-1.43498250636653,1.38725820055848,6.18513133238768));
#19437=CARTESIAN_POINT('Ctrl Pts',(-1.94350721947498,-0.454356464123216,
6.29633333333333));
#19438=CARTESIAN_POINT('Ctrl Pts',(-0.671238126752017,-1.8796540868244,
6.40753533427899));
#19439=CARTESIAN_POINT('Ctrl Pts',(1.21607200430908,-1.58266515362831,6.51873733522465));
#19440=CARTESIAN_POINT('Ctrl Pts',(1.98912154972485,0.164485771797453,6.6299393361703));
#19441=CARTESIAN_POINT('Ctrl Pts',(0.939581860845384,1.76092192816482,6.74114133711596));
#19442=CARTESIAN_POINT('Ctrl Pts',(-0.970876450125151,1.7438632468323,6.85234333806161));
#19443=CARTESIAN_POINT('Ctrl Pts',(-1.99174158107482,0.128940235259636,
6.96354533900727));
#19444=CARTESIAN_POINT('Ctrl Pts',(-1.18761679874002,-1.60412794320875,
7.07474733995293));
#19445=CARTESIAN_POINT('Ctrl Pts',(0.704695675764305,-1.86736822484612,
7.18594934089858));
#19446=CARTESIAN_POINT('Ctrl Pts',(1.95131068329089,-0.419579244957874,
7.29715134184424));
#19447=CARTESIAN_POINT('Ctrl Pts',(1.4099817335776,1.4126612047182,7.40835334278989));
#19448=CARTESIAN_POINT('Ctrl Pts',(-0.423283099660761,1.95051053364244,
7.51955534373554));
#19449=CARTESIAN_POINT('Ctrl Pts',(-1.86870276570027,0.701149232434471,
7.63075734468121));
#19450=CARTESIAN_POINT('Ctrl Pts',(-1.60187029707667,-1.19066031684572,
7.74195934562685));
#19451=CARTESIAN_POINT('Ctrl Pts',(0.132721349865937,-1.99149287614267,
7.85316134657253));
#19452=CARTESIAN_POINT('Ctrl Pts',(1.7457034228491,-0.967564522299928,7.96436334751815));
#19453=CARTESIAN_POINT('Ctrl Pts',(1.75913478124116,0.942924489928461,8.07556534846384));
#19454=CARTESIAN_POINT('Ctrl Pts',(0.160709337035842,1.98942805177203,8.18676734940947));
#19455=CARTESIAN_POINT('Ctrl Pts',(-1.58497158087089,1.21306924946704,8.29796935035515));
#19456=CARTESIAN_POINT('Ctrl Pts',(-1.87837532998656,-0.674813464785299,
8.4091713513008));
#19457=CARTESIAN_POINT('Ctrl Pts',(-0.45066773734148,-1.94435116675061,
8.52037335224644));
#19458=CARTESIAN_POINT('Ctrl Pts',(1.38998369362979,-1.4323750376837,8.63157535319211));
#19459=CARTESIAN_POINT('Ctrl Pts',(1.95701024929279,0.392156930733598,8.74277735413776));
#19460=CARTESIAN_POINT('Ctrl Pts',(0.730894753810015,1.8571707504813,8.85397935508342));
#19461=CARTESIAN_POINT('Ctrl Pts',(-1.16497011981623,1.62086699364572,8.96518135602907));
#19462=CARTESIAN_POINT('Ctrl Pts',(-1.99330988858858,-0.101303439668302,
9.07638335697474));
#19463=CARTESIAN_POINT('Ctrl Pts',(-0.995390299867974,-1.72931333772327,
9.18758535792038));
#19464=CARTESIAN_POINT('Ctrl Pts',(0.914901585160197,-1.7753658866198,9.29878735886605));
#19465=CARTESIAN_POINT('Ctrl Pts',(1.98629639100309,-0.189557281901872,
9.40998935981169));
#19466=CARTESIAN_POINT('Ctrl Pts',(1.4879659438757,0.975690954768368,9.4841240271088));
#19467=CARTESIAN_POINT('Ctrl Pts',(1.04739234074599,1.3241747350675,9.52119136075735));
#19468=CARTESIAN_POINT('Ctrl Pts',(-0.802959149489929,1.63459616787395,
-0.0766913607573553));
#19469=CARTESIAN_POINT('Ctrl Pts',(-1.34681480861903,1.36743912561342,-0.0396240271088033));
#19470=CARTESIAN_POINT('Ctrl Pts',(-2.13747526583221,0.252240694356305,
0.0345106401883006));
#19471=CARTESIAN_POINT('Ctrl Pts',(-1.3687595734217,-1.66368268602643,0.145712641133957));
#19472=CARTESIAN_POINT('Ctrl Pts',(0.655913749241891,-2.04993357112408,
0.256914642079612));
#19473=CARTESIAN_POINT('Ctrl Pts',(2.07866639915472,-0.560517465896349,
0.368116643025269));
#19474=CARTESIAN_POINT('Ctrl Pts',(1.59726310517123,1.44386175018322,0.479318643970924));
#19475=CARTESIAN_POINT('Ctrl Pts',(-0.347930429331078,2.12454229357336,
0.590520644916581));
#19476=CARTESIAN_POINT('Ctrl Pts',(-1.97419027428688,0.858927959588711,
0.701722645862234));
#19477=CARTESIAN_POINT('Ctrl Pts',(-1.79161167711204,-1.19390174267229,
0.812924646807894));
#19478=CARTESIAN_POINT('Ctrl Pts',(0.0326186498214368,-2.15268093522164,
0.924126647753546));
#19479=CARTESIAN_POINT('Ctrl Pts',(1.82694202515831,-1.13905958962419,1.03532864869921));
#19480=CARTESIAN_POINT('Ctrl Pts',(1.94728784548518,0.918286214270224,1.14653064964486));
#19481=CARTESIAN_POINT('Ctrl Pts',(0.283370464226838,2.13421107384081,1.25773265059052));
#19482=CARTESIAN_POINT('Ctrl Pts',(-1.6401903926881,1.39461220321543,1.36893465153617));
#19483=CARTESIAN_POINT('Ctrl Pts',(-2.06088157770847,-0.622843945347137,
1.48013665248183));
#19484=CARTESIAN_POINT('Ctrl Pts',(-0.593230594706847,-2.06959942077943,
1.59133865342748));
#19485=CARTESIAN_POINT('Ctrl Pts',(1.4179844030896,-1.6200266672553,1.70254065437314));
#19486=CARTESIAN_POINT('Ctrl Pts',(2.1299310441116,0.313942230517263,1.81374265531879));
#19487=CARTESIAN_POINT('Ctrl Pts',(0.890267633152099,1.96025230845148,1.92494465626445));
#19488=CARTESIAN_POINT('Ctrl Pts',(-1.16512877720859,1.81042558198,2.03614665721011));
#19489=CARTESIAN_POINT('Ctrl Pts',(-2.15294281420147,0.00174480076089232,
2.14734865815576));
#19490=CARTESIAN_POINT('Ctrl Pts',(-1.16806170472066,-1.80853465810824,
2.25855065910142));
#19491=CARTESIAN_POINT('Ctrl Pts',(0.88708917857608,-1.96169278609528,2.36975266004707));
#19492=CARTESIAN_POINT('Ctrl Pts',(2.12941935815555,-0.317394052653655,
2.48095466099273));
#19493=CARTESIAN_POINT('Ctrl Pts',(1.42060844111238,1.61772600856275,2.59215666193839));
#19494=CARTESIAN_POINT('Ctrl Pts',(-0.589875392140936,2.07055857430028,
2.70335866288404));
#19495=CARTESIAN_POINT('Ctrl Pts',(-2.05986910899239,0.626182912413284,
2.8145606638297));
#19496=CARTESIAN_POINT('Ctrl Pts',(-1.64244912653854,-1.39195066438994,
2.92576266477535));
#19497=CARTESIAN_POINT('Ctrl Pts',(0.2799116152051,-2.13466982784364,3.03696466572101));
#19498=CARTESIAN_POINT('Ctrl Pts',(1.94579537278442,-0.921437004443841,
3.14816666666667));
#19499=CARTESIAN_POINT('Ctrl Pts',(1.8287887389056,1.13608870001637,3.25936866761232));
#19500=CARTESIAN_POINT('Ctrl Pts',(0.0361023721692252,2.15264079787999,
3.37057066855798));
#19501=CARTESIAN_POINT('Ctrl Pts',(-1.78966382062389,1.19677449633167,3.48177266950363));
#19502=CARTESIAN_POINT('Ctrl Pts',(-1.97559960047322,-0.855670499974885,
3.59297467044929));
#19503=CARTESIAN_POINT('Ctrl Pts',(-0.351336017011034,-2.12408304665435,
3.70417667139495));
#19504=CARTESIAN_POINT('Ctrl Pts',(1.59484919174131,-1.44624404632384,3.8153786723406));
#19505=CARTESIAN_POINT('Ctrl Pts',(2.0797084360703,0.556757224347788,3.92658067328626));
#19506=CARTESIAN_POINT('Ctrl Pts',(0.658975633330173,2.04961384182598,4.03778267423191));
#19507=CARTESIAN_POINT('Ctrl Pts',(-1.36556234916871,1.66445344076038,4.14898467517757));
#19508=CARTESIAN_POINT('Ctrl Pts',(-2.1388649626988,-0.245809798962268,
4.26018667612322));
#19509=CARTESIAN_POINT('Ctrl Pts',(-0.952371677926902,-1.93084281416416,
4.37138867706889));
#19510=CARTESIAN_POINT('Ctrl Pts',(1.10675926308356,-1.846686145371,4.48259067801454));
#19511=CARTESIAN_POINT('Ctrl Pts',(2.15179052878673,-0.0704507356260967,
4.59379267896019));
#19512=CARTESIAN_POINT('Ctrl Pts',(1.2251824783732,1.7703371658003,4.70499467990585));
#19513=CARTESIAN_POINT('Ctrl Pts',(-0.824033888910251,1.98900325184601,
4.8161966808515));
#19514=CARTESIAN_POINT('Ctrl Pts',(-2.11820575188311,0.385188497512356,
4.92739868179717));
#19515=CARTESIAN_POINT('Ctrl Pts',(-1.47151130646485,-1.57156618087582,
5.03860068274281));
#19516=CARTESIAN_POINT('Ctrl Pts',(0.523497255556681,-2.08832861622669,
5.14980268368848));
#19517=CARTESIAN_POINT('Ctrl Pts',(2.03883655743106,-0.691600519092537,
5.26100468463412));
#19518=CARTESIAN_POINT('Ctrl Pts',(1.68603383433167,1.33882623794692,5.37220668557979));
#19519=CARTESIAN_POINT('Ctrl Pts',(-0.211645377254637,2.14251534888651,
5.48340868652544));
#19520=CARTESIAN_POINT('Ctrl Pts',(-1.91539848809492,0.983063791281674,
5.5946106874711));
#19521=CARTESIAN_POINT('Ctrl Pts',(-1.86411321827678,-1.07714794497825,
5.70581268841674));
#19522=CARTESIAN_POINT('Ctrl Pts',(-0.104781155948357,-2.15039221894326,
5.81701468936241));
#19523=CARTESIAN_POINT('Ctrl Pts',(1.75055962279115,-1.25327841797843,5.92821669030807));
#19524=CARTESIAN_POINT('Ctrl Pts',(2.00190032284059,0.792187404173254,6.03941869125372));
#19525=CARTESIAN_POINT('Ctrl Pts',(0.418942874133682,2.11178897008822,6.15062069219938));
#19526=CARTESIAN_POINT('Ctrl Pts',(-1.54788290691678,1.49640378652543,6.26182269314503));
#19527=CARTESIAN_POINT('Ctrl Pts',(-2.09641691877623,-0.490103956907626,
6.37302469409069));
#19528=CARTESIAN_POINT('Ctrl Pts',(-0.724049260712674,-2.02754000066438,
6.48422669503635));
#19529=CARTESIAN_POINT('Ctrl Pts',(1.31174914028481,-1.70718481082889,6.59542869598199));
#19530=CARTESIAN_POINT('Ctrl Pts',(2.14562005664793,0.177427051177754,6.70663069692766));
#19531=CARTESIAN_POINT('Ctrl Pts',(1.01350552748841,1.89946632863346,6.81783269787331));
#19532=CARTESIAN_POINT('Ctrl Pts',(-1.04726228731662,1.88106551807864,6.92903469881897));
#19533=CARTESIAN_POINT('Ctrl Pts',(-2.14844622471911,0.13908489147899,7.04023669976463));
#19534=CARTESIAN_POINT('Ctrl Pts',(-1.28105515891731,-1.73033623252141,
7.15143870071027));
#19535=CARTESIAN_POINT('Ctrl Pts',(0.760139155881188,-2.01428752150974,
7.26264070165595));
#19536=CARTESIAN_POINT('Ctrl Pts',(2.10483433724774,-0.452590563638184,
7.37384270260158));
#19537=CARTESIAN_POINT('Ctrl Pts',(1.52091514341585,1.52380542783373,7.48504470354725));
#19538=CARTESIAN_POINT('Ctrl Pts',(-0.456585827245116,2.10397123406821,
7.59624670449291));
#19539=CARTESIAN_POINT('Ctrl Pts',(-2.01572706029682,0.756313688332832,
7.70744870543855));
#19540=CARTESIAN_POINT('Ctrl Pts',(-1.72790096112112,-1.28433813249488,
7.81865070638422));
#19541=CARTESIAN_POINT('Ctrl Pts',(0.143163493581931,-2.14817795238016,
7.92985270732987));
#19542=CARTESIAN_POINT('Ctrl Pts',(1.88305047398539,-1.0436897862953,8.04105470827553));
#19543=CARTESIAN_POINT('Ctrl Pts',(1.89753857400022,1.01711114525648,8.15225670922118));
#19544=CARTESIAN_POINT('Ctrl Pts',(0.173353497116561,2.14595067341688,8.26345871016684));
#19545=CARTESIAN_POINT('Ctrl Pts',(-1.7096727013007,1.30851013711022,8.3746607111125));
#19546=CARTESIAN_POINT('Ctrl Pts',(-2.02616063482361,-0.72790589631874,
8.48586271205815));
#19547=CARTESIAN_POINT('Ctrl Pts',(-0.486125011444274,-2.09732726545744,
8.59706471300382));
#19548=CARTESIAN_POINT('Ctrl Pts',(1.49934371375051,-1.54507028990818,8.70826671394946));
#19549=CARTESIAN_POINT('Ctrl Pts',(2.11098232912363,0.423010738610651,8.81946871489512));
#19550=CARTESIAN_POINT('Ctrl Pts',(0.788399503937036,2.00328773845105,8.93067071584077));
#19551=CARTESIAN_POINT('Ctrl Pts',(-1.25662670278695,1.74839226451795,9.04187271678643));
#19552=CARTESIAN_POINT('Ctrl Pts',(-2.15013792227122,-0.109273710291747,
9.15307471773208));
#19553=CARTESIAN_POINT('Ctrl Pts',(-1.07370481803134,-1.86537086291235,
9.26427671867775));
#19554=CARTESIAN_POINT('Ctrl Pts',(0.986883476904773,-1.91504669724527,
9.37547871962339));
#19555=CARTESIAN_POINT('Ctrl Pts',(2.14257262235841,-0.204471117407888,
9.48668072056906));
#19556=CARTESIAN_POINT('Ctrl Pts',(1.60503493274727,1.05245558368745,9.56081538786616));
#19557=CARTESIAN_POINT('Ctrl Pts',(1.12979823369512,1.42835709082749,9.59788272151471));
#19558=CARTESIAN_POINT('Ctrl Pts',(-0.861525859670525,1.75382131162755,
0.));
#19559=CARTESIAN_POINT('Ctrl Pts',(-1.44504958508734,1.46717821073413,0.037067333648552));
#19560=CARTESIAN_POINT('Ctrl Pts',(-2.29337970317716,0.270638775568176,
0.111202000945656));
#19561=CARTESIAN_POINT('Ctrl Pts',(-1.46859497014699,-1.78502935947413,
0.222404001891312));
#19562=CARTESIAN_POINT('Ctrl Pts',(0.703755174898128,-2.19945284047394,
0.333606002836967));
#19563=CARTESIAN_POINT('Ctrl Pts',(2.23028140053902,-0.601400820917812,
0.444808003782624));
#19564=CARTESIAN_POINT('Ctrl Pts',(1.71376522787844,1.54917499397346,0.556010004728279));
#19565=CARTESIAN_POINT('Ctrl Pts',(-0.373307985126514,2.27950341812521,
0.667212005673936));
#19566=CARTESIAN_POINT('Ctrl Pts',(-2.11818493417584,0.921576956000567,
0.778414006619591));
#19567=CARTESIAN_POINT('Ctrl Pts',(-1.92228931110658,-1.28098325533905,
0.889616007565248));
#19568=CARTESIAN_POINT('Ctrl Pts',(0.0349978082279097,-2.30969445268953,
1.0008180085109));
#19569=CARTESIAN_POINT('Ctrl Pts',(1.96019660501108,-1.22214099283922,1.11202000945656));
#19570=CARTESIAN_POINT('Ctrl Pts',(2.08932028008312,0.985264718230436,1.22322201040222));
#19571=CARTESIAN_POINT('Ctrl Pts',(0.304039107037209,2.28987742561633,1.33442401134787));
#19572=CARTESIAN_POINT('Ctrl Pts',(-1.75982357132563,1.49633325436971,1.44562601229353));
#19573=CARTESIAN_POINT('Ctrl Pts',(-2.21119937924903,-0.668273306053786,
1.55682801323918));
#19574=CARTESIAN_POINT('Ctrl Pts',(-0.636499999299278,-2.22055308952301,
1.66803001418484));
#19575=CARTESIAN_POINT('Ctrl Pts',(1.52141018960579,-1.73818913214068,1.77923201513049));
#19576=CARTESIAN_POINT('Ctrl Pts',(2.28528521654291,0.33684073493038,1.89043401607615));
#19577=CARTESIAN_POINT('Ctrl Pts',(0.955202501242366,2.1032303527304,2.0016360170218));
#19578=CARTESIAN_POINT('Ctrl Pts',(-1.25011163027303,1.94247547571461,2.11283801796746));
#19579=CARTESIAN_POINT('Ctrl Pts',(-2.30997543275355,0.00187206407255709,
2.22404001891312));
#19580=CARTESIAN_POINT('Ctrl Pts',(-1.25325848138969,-1.94044663051715,
2.33524201985877));
#19581=CARTESIAN_POINT('Ctrl Pts',(0.951792214663295,-2.10477589678604,
2.44644402080443));
#19582=CARTESIAN_POINT('Ctrl Pts',(2.28473620893343,-0.340544328114909,
2.55764602175008));
#19583=CARTESIAN_POINT('Ctrl Pts',(1.52422562126857,1.73572066664131,2.66884802269574));
#19584=CARTESIAN_POINT('Ctrl Pts',(-0.632900072980707,2.22158220235165,
2.7800500236414));
#19585=CARTESIAN_POINT('Ctrl Pts',(-2.21011306248986,0.671855812678093,
2.89125202458705));
#19586=CARTESIAN_POINT('Ctrl Pts',(-1.76224705404392,-1.49347758664845,
3.00245402553271));
#19587=CARTESIAN_POINT('Ctrl Pts',(0.300327974436209,-2.29036964049042,
3.11365602647836));
#19588=CARTESIAN_POINT('Ctrl Pts',(2.08771894852425,-0.988645322604533,
3.22485802742402));
#19589=CARTESIAN_POINT('Ctrl Pts',(1.96217801545981,1.21895341072497,3.33606002836968));
#19590=CARTESIAN_POINT('Ctrl Pts',(0.0387356283803547,2.30965138778668,
3.44726202931533));
#19591=CARTESIAN_POINT('Ctrl Pts',(-1.92019938070783,1.2840655436069,3.55846403026099));
#19592=CARTESIAN_POINT('Ctrl Pts',(-2.11969705463056,-0.918081901867433,
3.66966603120664));
#19593=CARTESIAN_POINT('Ctrl Pts',(-0.37696197157843,-2.27901067438232,
3.7808680321523));
#19594=CARTESIAN_POINT('Ctrl Pts',(1.71117524700055,-1.55173105144146,3.89207003309796));
#19595=CARTESIAN_POINT('Ctrl Pts',(2.23139944216054,0.597366312643301,4.00327203404361));
#19596=CARTESIAN_POINT('Ctrl Pts',(0.707040388502159,2.19910979057086,4.11447403498927));
#19597=CARTESIAN_POINT('Ctrl Pts',(-1.46516454485713,1.78585633197353,4.22567603593493));
#19598=CARTESIAN_POINT('Ctrl Pts',(-2.29487076257717,-0.263738819715705,
4.33687803688058));
#19599=CARTESIAN_POINT('Ctrl Pts',(-1.0218363276302,-2.07167577132429,4.44808003782624));
#19600=CARTESIAN_POINT('Ctrl Pts',(1.18748472594413,-1.98138083356179,4.55928203877189));
#19601=CARTESIAN_POINT('Ctrl Pts',(2.30873910126252,-0.0755893131216698,
4.67048403971755));
#19602=CARTESIAN_POINT('Ctrl Pts',(1.31454556387366,1.89946306688411,4.78168604066321));
#19603=CARTESIAN_POINT('Ctrl Pts',(-0.884137760920989,2.13407834946853,
4.89288804160886));
#19604=CARTESIAN_POINT('Ctrl Pts',(-2.27270469800289,0.413283604359384,
5.00409004255452));
#19605=CARTESIAN_POINT('Ctrl Pts',(-1.57884126997291,-1.68619400609389,
5.11529204350018));
#19606=CARTESIAN_POINT('Ctrl Pts',(0.561680408542726,-2.24064836612444,
5.22649404444582));
#19607=CARTESIAN_POINT('Ctrl Pts',(2.18754642622144,-0.74204488751176,5.33769604539148));
#19608=CARTESIAN_POINT('Ctrl Pts',(1.80901076907701,1.4364783393145,5.44889804633715));
#19609=CARTESIAN_POINT('Ctrl Pts',(-0.227082493175914,2.29878740279542,
5.56010004728278));
#19610=CARTESIAN_POINT('Ctrl Pts',(-2.0551049578498,1.05476708053322,5.67130204822846));
#19611=CARTESIAN_POINT('Ctrl Pts',(-2.00007901263631,-1.15571359997482,
5.7825040491741));
#19612=CARTESIAN_POINT('Ctrl Pts',(-0.112423745981393,-2.30723880066723,
5.89370605011977));
#19613=CARTESIAN_POINT('Ctrl Pts',(1.87824297772521,-1.34469078176803,6.00490805106541));
#19614=CARTESIAN_POINT('Ctrl Pts',(2.14791611466854,0.849968438411925,6.11611005201108));
#19615=CARTESIAN_POINT('Ctrl Pts',(0.449499977701421,2.26581988517564,6.22731205295673));
#19616=CARTESIAN_POINT('Ctrl Pts',(-1.66078330746703,1.60554937249238,6.33851405390239));
#19617=CARTESIAN_POINT('Ctrl Pts',(-2.24932661807747,-0.525851449692036,
6.44971605484804));
#19618=CARTESIAN_POINT('Ctrl Pts',(-0.776860394673336,-2.17542591450436,
6.5609180557937));
#19619=CARTESIAN_POINT('Ctrl Pts',(1.40742627626055,-1.83170446802946,6.67212005673936));
#19620=CARTESIAN_POINT('Ctrl Pts',(2.302118563571,0.190368330558053,6.783322057685));
#19621=CARTESIAN_POINT('Ctrl Pts',(1.08742919413144,2.0380107291021,6.89452405863067));
#19622=CARTESIAN_POINT('Ctrl Pts',(-1.1236481245081,2.01826778932498,7.00572605957632));
#19623=CARTESIAN_POINT('Ctrl Pts',(-2.30515086836339,0.149229547698346,
7.11692806052198));
#19624=CARTESIAN_POINT('Ctrl Pts',(-1.3744935190946,-1.85654452183408,7.22813006146763));
#19625=CARTESIAN_POINT('Ctrl Pts',(0.815582635998072,-2.16120681817335,
7.33933206241329));
#19626=CARTESIAN_POINT('Ctrl Pts',(2.25835799120458,-0.485601882318497,
7.45053406335894));
#19627=CARTESIAN_POINT('Ctrl Pts',(1.6318485532541,1.63494965094926,7.5617360643046));
#19628=CARTESIAN_POINT('Ctrl Pts',(-0.489888554829468,2.25743193449398,
7.67293806525026));
#19629=CARTESIAN_POINT('Ctrl Pts',(-2.16275135489337,0.811478144231195,
7.78414006619591));
#19630=CARTESIAN_POINT('Ctrl Pts',(-1.85393162516556,-1.37801594814403,
7.89534206714158));
#19631=CARTESIAN_POINT('Ctrl Pts',(0.153605637297925,-2.30486302861764,
8.00654406808722));
#19632=CARTESIAN_POINT('Ctrl Pts',(2.02039752512168,-1.11981505029068,8.11774606903289));
#19633=CARTESIAN_POINT('Ctrl Pts',(2.03594236675928,1.09129780058451,8.22894806997853));
#19634=CARTESIAN_POINT('Ctrl Pts',(0.185997657197281,2.30247329506172,8.3401500709242));
#19635=CARTESIAN_POINT('Ctrl Pts',(-1.83437382173052,1.40395102475339,8.45135207186985));
#19636=CARTESIAN_POINT('Ctrl Pts',(-2.17394593966066,-0.78099832785218,
8.56255407281551));
#19637=CARTESIAN_POINT('Ctrl Pts',(-0.521582285547066,-2.25030336416427,
8.67375607376116));
#19638=CARTESIAN_POINT('Ctrl Pts',(1.60870373387123,-1.65776554213267,8.78495807470682));
#19639=CARTESIAN_POINT('Ctrl Pts',(2.26495440895447,0.453864546487703,8.89616007565248));
#19640=CARTESIAN_POINT('Ctrl Pts',(0.845904254064056,2.14940472642079,9.00736207659812));
#19641=CARTESIAN_POINT('Ctrl Pts',(-1.34828328575767,1.87591753539018,9.11856407754379));
#19642=CARTESIAN_POINT('Ctrl Pts',(-2.30696595595385,-0.117243980915191,
9.22976607848944));
#19643=CARTESIAN_POINT('Ctrl Pts',(-1.1520193361947,-2.00142838810143,9.34096807943509));
#19644=CARTESIAN_POINT('Ctrl Pts',(1.05886536864935,-2.05472750787074,9.45217008038076));
#19645=CARTESIAN_POINT('Ctrl Pts',(2.29884885371374,-0.219384952913903,
9.5633720813264));
#19646=CARTESIAN_POINT('Ctrl Pts',(1.72210392161884,1.12922021260653,9.63750674862351));
#19647=CARTESIAN_POINT('Ctrl Pts',(1.21220412664425,1.53253944658748,9.67457408227206));
#19648=CARTESIAN_POINT('Ctrl Pts',(-1.95199070173634,-0.00143915622514865,
8.52413030787577));
#19649=CARTESIAN_POINT('Ctrl Pts',(-1.95352332736863,-0.226597580633425,
8.53693822952235));
#19650=CARTESIAN_POINT('Ctrl Pts',(-1.91755839154915,-0.451281101938663,
8.54974615116893));
#19651=CARTESIAN_POINT('Ctrl Pts',(-1.84195664432004,-0.661724275136593,
8.56255407281551));
#19652=CARTESIAN_POINT('Ctrl Pts',(-1.62315805495613,-1.27076667328954,
8.59962140646406));
#19653=CARTESIAN_POINT('Ctrl Pts',(-1.0723701702516,-1.76053501872691,8.63668874011261));
#19654=CARTESIAN_POINT('Ctrl Pts',(-0.441928557996276,-1.90666288777366,
8.67375607376116));
#19655=CARTESIAN_POINT('Ctrl Pts',(0.188513054259035,-2.0527907568204,8.71082340740971));
#19656=CARTESIAN_POINT('Ctrl Pts',(0.898608394065125,-1.85527814947654,
8.74789074105826));
#19657=CARTESIAN_POINT('Ctrl Pts',(1.36303117648205,-1.40458349770121,8.78495807470682));
#19658=CARTESIAN_POINT('Ctrl Pts',(1.82745395889897,-0.95388884592588,8.82202540835537));
#19659=CARTESIAN_POINT('Ctrl Pts',(2.04620418392672,-0.250012149719083,
8.85909274200392));
#19660=CARTESIAN_POINT('Ctrl Pts',(1.91907093729219,0.384516228373164,8.89616007565247));
#19661=CARTESIAN_POINT('Ctrl Pts',(1.79193769065766,1.01904460646541,8.93322740930103));
#19662=CARTESIAN_POINT('Ctrl Pts',(1.31892097236085,1.58422466644311,8.97029474294957));
#19663=CARTESIAN_POINT('Ctrl Pts',(0.716714689908818,1.82123349792685,9.00736207659813));
#19664=CARTESIAN_POINT('Ctrl Pts',(0.507473848776133,1.90358389628803,9.02024138439875));
#19665=CARTESIAN_POINT('Ctrl Pts',(0.282636413049304,1.9463153545146,9.03312069219937));
#19666=CARTESIAN_POINT('Ctrl Pts',(0.0562592026297114,1.95117115182352,
9.046));
#19667=CARTESIAN_POINT('Ctrl Pts',(-0.905550660636153,-1.26792405592273,
1.45716771982052E-16));
#19668=CARTESIAN_POINT('Ctrl Pts',(-0.937331646933896,-1.25093119319315,
1.27175061552484E-16));
#19669=CARTESIAN_POINT('Ctrl Pts',(-0.968423391396878,-1.23278887404085,
4.27877505352727E-17));
#19670=CARTESIAN_POINT('Ctrl Pts',(-0.998756220109605,-1.21351103938415,
8.67361737988404E-19));
#19671=CARTESIAN_POINT('Ctrl Pts',(-1.04879905844205,-1.1817066345836,-4.27343170489691E-17));
#19672=CARTESIAN_POINT('Ctrl Pts',(-1.09677754676758,-1.14681449344115,
3.59228313652207E-16));
#19673=CARTESIAN_POINT('Ctrl Pts',(-1.14261320333336,-1.1091553561269,4.82253126321552E-16));
#19674=CARTESIAN_POINT('Ctrl Pts',(-1.16875585300247,-1.08767623468714,
5.52421087668592E-16));
#19675=CARTESIAN_POINT('Ctrl Pts',(-1.19420116520872,-1.06529603829454,
1.68485755535521E-16));
#19676=CARTESIAN_POINT('Ctrl Pts',(-1.21893184621838,-1.04206746474762,
1.70002900645727E-16));
#19677=CARTESIAN_POINT('Ctrl Pts',(-1.23255995383574,-1.02926710959479,
1.70838939767535E-16));
#19678=CARTESIAN_POINT('Ctrl Pts',(-1.24597488110422,-1.01620487704946,
4.21475736447755E-16));
#19679=CARTESIAN_POINT('Ctrl Pts',(-1.25915060380592,-1.0029128321029,4.02455846426619E-16));
#19680=CARTESIAN_POINT('Ctrl Pts',(-1.30303064134819,-0.95864539839369,
3.39112566739263E-16));
#19681=CARTESIAN_POINT('Ctrl Pts',(-1.34430260426558,-0.91179514360288,
3.08161369943384E-16));
#19682=CARTESIAN_POINT('Ctrl Pts',(-1.38287779953103,-0.862711096565261,
2.84494650060196E-16));
#19683=CARTESIAN_POINT('Ctrl Pts',(-1.41251185733787,-0.825003977332371,
2.66313512147855E-16));
#19684=CARTESIAN_POINT('Ctrl Pts',(-1.44055413744545,-0.785977345707785,
2.85602281713357E-16));
#19685=CARTESIAN_POINT('Ctrl Pts',(-1.46695437986393,-0.745771217825177,
2.63677968348475E-16));
#19686=CARTESIAN_POINT('Ctrl Pts',(-1.48000187887279,-0.725900589162651,
2.52842558113835E-16));
#19687=CARTESIAN_POINT('Ctrl Pts',(-1.49264815413029,-0.705741645745626,
3.81368532133475E-16));
#19688=CARTESIAN_POINT('Ctrl Pts',(-1.50488615061787,-0.685310125526541,
3.53883589099269E-16));
#19689=CARTESIAN_POINT('Ctrl Pts',(-1.51114001186157,-0.674869209599035,
3.398382328842E-16));
#19690=CARTESIAN_POINT('Ctrl Pts',(-1.51728238793534,-0.664365181000008,
3.54964001115812E-16));
#19691=CARTESIAN_POINT('Ctrl Pts',(-1.52331182355158,-0.653802123157991,
3.53883589099269E-16));
#19692=CARTESIAN_POINT('Ctrl Pts',(-1.55543280121804,-0.597528905127582,
3.48127844704137E-16));
#19693=CARTESIAN_POINT('Ctrl Pts',(-1.5843593035114,-0.539569562213937,
2.67786881775446E-16));
#19694=CARTESIAN_POINT('Ctrl Pts',(-1.60999744801157,-0.480277394578745,
2.4980018054066E-16));
#19695=CARTESIAN_POINT('Ctrl Pts',(-1.6361318010197,-0.419837668155283,
2.31465359176401E-16));
#19696=CARTESIAN_POINT('Ctrl Pts',(-1.65885002952378,-0.358012230099105,
4.67501104767292E-16));
#19697=CARTESIAN_POINT('Ctrl Pts',(-1.67801828739638,-0.295134384099341,
4.57966997657877E-16));
#19698=CARTESIAN_POINT('Ctrl Pts',(-1.69037417655557,-0.254603225717345,
4.51821297226535E-16));
#19699=CARTESIAN_POINT('Ctrl Pts',(-1.70125428685937,-0.213633977893128,
1.06733149524263E-17));
#19700=CARTESIAN_POINT('Ctrl Pts',(-1.71061315113863,-0.172309644008052,
-5.55111512312578E-17));
#19701=CARTESIAN_POINT('Ctrl Pts',(-1.71583359551538,-0.149258622001936,
-9.24293406618695E-17));
#19702=CARTESIAN_POINT('Ctrl Pts',(-1.7205805610286,-0.126097041535353,
3.62932093827782E-16));
#19703=CARTESIAN_POINT('Ctrl Pts',(-1.72484497590278,-0.102838875523928,
3.60822483003176E-16));
#19704=CARTESIAN_POINT('Ctrl Pts',(-1.72698171347111,-0.0911850851322128,
3.59765436529865E-16));
#19705=CARTESIAN_POINT('Ctrl Pts',(-1.72899754888149,-0.0795054094991753,
1.33624776520754E-16));
#19706=CARTESIAN_POINT('Ctrl Pts',(-1.73089043201219,-0.0678066984905219,
1.38777878078145E-16));
#19707=CARTESIAN_POINT('Ctrl Pts',(-1.74172160283504,-0.000866095931865457,
1.68264179863231E-16));
#19708=CARTESIAN_POINT('Ctrl Pts',(-1.748486900033,0.0664195158076909,2.42458198468553E-16));
#19709=CARTESIAN_POINT('Ctrl Pts',(-1.75106690168969,0.133692207227197,
2.22044604925031E-16));
#19710=CARTESIAN_POINT('Ctrl Pts',(-1.75197579459359,0.157391289628443,
2.14853225699892E-16));
#19711=CARTESIAN_POINT('Ctrl Pts',(-1.7523649021625,0.181089059905603,-1.04868588637259E-16));
#19712=CARTESIAN_POINT('Ctrl Pts',(-1.75222770108741,0.204770690960275,
-9.71445146547012E-17));
#19713=CARTESIAN_POINT('Ctrl Pts',(-1.75185206838866,0.269606881041249,
-6.21195546873158E-17));
#19714=CARTESIAN_POINT('Ctrl Pts',(-1.74753527769623,0.334321428897923,
1.54729584489575E-16));
#19715=CARTESIAN_POINT('Ctrl Pts',(-1.73949435710187,0.398678851668467,
8.32667268468867E-17));
#19716=CARTESIAN_POINT('Ctrl Pts',(-1.7312762859938,0.46445414076046,1.02294621704162E-17));
#19717=CARTESIAN_POINT('Ctrl Pts',(-1.71916809095178,0.529857212284545,
-1.51627889474086E-16));
#19718=CARTESIAN_POINT('Ctrl Pts',(-1.70334767938921,0.594640505552203,
-1.66533453693773E-16));
#19719=CARTESIAN_POINT('Ctrl Pts',(-1.70064831213801,0.605694193983744,
-1.69076724566096E-16));
#19720=CARTESIAN_POINT('Ctrl Pts',(-1.69784071539616,0.616729589129694,
5.32060987810746E-16));
#19721=CARTESIAN_POINT('Ctrl Pts',(-1.69492950185833,0.627731892802461,
5.27355936696949E-16));
#19722=CARTESIAN_POINT('Ctrl Pts',(-1.67758049779776,0.693298711798846,
4.9931678744945E-16));
#19723=CARTESIAN_POINT('Ctrl Pts',(-1.65652692130866,0.757811857431264,
1.02969912804589E-16));
#19724=CARTESIAN_POINT('Ctrl Pts',(-1.63202614811433,0.82101547035702,8.32667268468867E-17));
#19725=CARTESIAN_POINT('Ctrl Pts',(-1.60700935125733,0.885550247796537,
6.31485617330762E-17));
#19726=CARTESIAN_POINT('Ctrl Pts',(-1.57839845257882,0.948720629503181,
8.44128967647446E-17));
#19727=CARTESIAN_POINT('Ctrl Pts',(-1.54641225600304,1.01025741355839,1.94289029309402E-16));
#19728=CARTESIAN_POINT('Ctrl Pts',(-1.51418344328006,1.07226095574858,3.04998575226134E-16));
#19729=CARTESIAN_POINT('Ctrl Pts',(-1.47852761223994,1.13260700774386,2.72099366666861E-16));
#19730=CARTESIAN_POINT('Ctrl Pts',(-1.43961707028964,1.19100921034501,4.16333634234434E-16));
#19731=CARTESIAN_POINT('Ctrl Pts',(-1.42987064738873,1.20563795968555,4.52461842633911E-16));
#19732=CARTESIAN_POINT('Ctrl Pts',(-1.41991978147756,1.22014465371079,-1.08678851106874E-16));
#19733=CARTESIAN_POINT('Ctrl Pts',(-1.40976671738967,1.23452457045435,-1.11022302462516E-16));
#19734=CARTESIAN_POINT('Ctrl Pts',(-1.40175176458173,1.24587625237856,-1.12872251587291E-16));
#19735=CARTESIAN_POINT('Ctrl Pts',(-1.39360965291877,1.25715028749333,2.28365264434682E-16));
#19736=CARTESIAN_POINT('Ctrl Pts',(-1.38535473796849,1.2683268547918,2.22044604925031E-16));
#19737=CARTESIAN_POINT('Ctrl Pts',(-1.34246203780014,1.32640051792846,1.89202334005651E-16));
#19738=CARTESIAN_POINT('Ctrl Pts',(-1.2964535599336,1.38195119811813,-1.79031912722901E-17));
#19739=CARTESIAN_POINT('Ctrl Pts',(-1.24757009345088,1.43469804908261,2.77555756156289E-17));
#19740=CARTESIAN_POINT('Ctrl Pts',(-1.19857852782046,1.48756154254492,7.35153106660103E-17));
#19741=CARTESIAN_POINT('Ctrl Pts',(-1.14669881160737,1.53760980197427,-1.09074190413862E-16));
#19742=CARTESIAN_POINT('Ctrl Pts',(-1.09212377872999,1.58454380591305,-1.38777878078145E-16));
#19743=CARTESIAN_POINT('Ctrl Pts',(-1.03871943285682,1.63047103027572,-1.67844393041064E-16));
#19744=CARTESIAN_POINT('Ctrl Pts',(-0.982733594885126,1.67341702936247,
5.10578859420299E-17));
#19745=CARTESIAN_POINT('Ctrl Pts',(-0.924307244265998,1.71307238365465,
8.32667268468867E-17));
#19746=CARTESIAN_POINT('Ctrl Pts',(-0.90368282336986,1.72707066882976,9.4636403103562E-17));
#19747=CARTESIAN_POINT('Ctrl Pts',(-0.882753967690277,1.74065858283188,
-3.60501930089703E-18));
#19748=CARTESIAN_POINT('Ctrl Pts',(-0.861525859670525,1.75382131162755,
0.));
#19749=CARTESIAN_POINT('Origin',(0.,0.,0.));
#19750=CARTESIAN_POINT('Origin',(-0.866025403784439,-1.5,-4.));
#19751=CARTESIAN_POINT('',(-0.866025403784439,-1.5,-4.));
#19752=CARTESIAN_POINT('',(0.866025403784439,-1.5,-4.));
#19753=CARTESIAN_POINT('',(-0.43301270189222,-1.5,-4.));
#19754=CARTESIAN_POINT('',(-0.866025403784439,-1.5,-2.));
#19755=CARTESIAN_POINT('',(-0.866025403784439,-1.5,-4.));
#19756=CARTESIAN_POINT('',(0.866025403784439,-1.5,-2.));
#19757=CARTESIAN_POINT('',(-0.866025403784439,-1.5,-2.));
#19758=CARTESIAN_POINT('',(0.866025403784439,-1.5,-4.));
#19759=CARTESIAN_POINT('Origin',(-1.73205080756888,2.12115047744981E-16,
-4.));
#19760=CARTESIAN_POINT('',(-1.73205080756888,2.12115047744981E-16,-4.));
#19761=CARTESIAN_POINT('',(-1.51554445662277,-0.375,-4.));
#19762=CARTESIAN_POINT('',(-1.73205080756888,2.77555756156289E-16,-2.));
#19763=CARTESIAN_POINT('',(-1.73205080756888,2.12115047744981E-16,-4.));
#19764=CARTESIAN_POINT('',(-1.73205080756888,2.12115047744981E-16,-2.));
#19765=CARTESIAN_POINT('Origin',(-0.866025403784438,1.5,-4.));
#19766=CARTESIAN_POINT('',(-0.866025403784438,1.5,-4.));
#19767=CARTESIAN_POINT('',(-1.08253175473055,1.125,-4.));
#19768=CARTESIAN_POINT('',(-0.866025403784438,1.5,-2.));
#19769=CARTESIAN_POINT('',(-0.866025403784438,1.5,-4.));
#19770=CARTESIAN_POINT('',(-0.866025403784438,1.5,-2.));
#19771=CARTESIAN_POINT('Origin',(0.866025403784439,1.5,-4.));
#19772=CARTESIAN_POINT('',(0.866025403784439,1.5,-4.));
#19773=CARTESIAN_POINT('',(0.43301270189222,1.5,-4.));
#19774=CARTESIAN_POINT('',(0.866025403784439,1.5,-2.));
#19775=CARTESIAN_POINT('',(0.866025403784439,1.5,-4.));
#19776=CARTESIAN_POINT('',(0.866025403784439,1.5,-2.));
#19777=CARTESIAN_POINT('Origin',(1.73205080756888,0.,-4.));
#19778=CARTESIAN_POINT('',(1.73205080756888,0.,-4.));
#19779=CARTESIAN_POINT('',(1.51554445662277,0.375,-4.));
#19780=CARTESIAN_POINT('',(1.73205080756888,0.,-2.));
#19781=CARTESIAN_POINT('',(1.73205080756888,0.,-4.));
#19782=CARTESIAN_POINT('',(1.73205080756888,0.,-2.));
#19783=CARTESIAN_POINT('Origin',(0.866025403784439,-1.5,-4.));
#19784=CARTESIAN_POINT('',(1.08253175473055,-1.125,-4.));
#19785=CARTESIAN_POINT('',(0.866025403784439,-1.5,-2.));
#19786=CARTESIAN_POINT('Origin',(0.,2.77555756156289E-16,-2.));
#19787=CARTESIAN_POINT('Origin',(0.,0.,0.));
#19788=CARTESIAN_POINT('',(-3.5,-4.28626379701574E-16,0.));
#19789=CARTESIAN_POINT('Origin',(0.,0.,0.));
#19790=CARTESIAN_POINT('Origin',(0.,0.,-4.));
#19791=CARTESIAN_POINT('',(-3.5,-4.28626379701574E-16,-4.));
#19792=CARTESIAN_POINT('',(-3.5,-4.28626379701574E-16,-4.));
#19793=CARTESIAN_POINT('Origin',(0.,0.,-4.));
#19794=CARTESIAN_POINT('Origin',(0.,0.,-4.));
#19795=CARTESIAN_POINT('Origin',(0.,0.,10.));
#19796=CARTESIAN_POINT('',(0.,0.,0.));
#19797=CARTESIAN_POINT('',(0.,0.,0.));
#19798=CARTESIAN_POINT('',(68.,-8.5774601177388E-16,1.53689128998124));
#19799=CARTESIAN_POINT('',(83.,-8.,-40.));
#19800=CARTESIAN_POINT('',(68.0789422237302,-8.,-38.4631087100188));
#19801=CARTESIAN_POINT('',(68.0789422237302,4.,-38.4631087100188));
#19802=CARTESIAN_POINT('',(98.,-8.57746011773878E-16,-1.53689128998124));
#19803=CARTESIAN_POINT('',(97.9210577762699,-8.,-41.5368912899813));
#19804=CARTESIAN_POINT('',(68.0789422237302,5.,-38.4631087100188));
#19805=CARTESIAN_POINT('',(83.,-14.,-40.));
#19806=CARTESIAN_POINT('',(83.,-10.,-40.));
#19807=CARTESIAN_POINT('',(97.9210577762699,4.,-41.5368912899813));
#19808=CARTESIAN_POINT('',(97.9210577762699,5.,-41.5368912899813));
#19809=CARTESIAN_POINT('',(83.,-8.,-40.));
#19810=CARTESIAN_POINT('',(83.,-4.,-40.));
#19811=CARTESIAN_POINT('',(83.,14.,-40.));
#19812=CARTESIAN_POINT('',(83.,-2.,-40.));
#19813=CARTESIAN_POINT('',(83.,16.,-40.));
#19814=CARTESIAN_POINT('',(83.,-14.,-65.));
#19815=CARTESIAN_POINT('',(83.,-10.,-65.));
#19816=CARTESIAN_POINT('',(83.,-4.,-65.));
#19817=CARTESIAN_POINT('',(83.,-3.,-65.));
#19818=CARTESIAN_POINT('',(77.8770290333959,2.,-89.7368592542325));
#19819=CARTESIAN_POINT('',(77.8770290333959,2.00000000000002,-89.7368592542326));
#19820=CARTESIAN_POINT('',(83.,-23.,-4.));
#19821=CARTESIAN_POINT('',(83.,23.,-4.));
#19822=UNCERTAINTY_MEASURE_WITH_UNIT(LENGTH_MEASURE(0.01),#19864,
'DISTANCE_ACCURACY_VALUE',
'Maximum model space distance between geometric entities at asserted c
onnectivities');
#19823=UNCERTAINTY_MEASURE_WITH_UNIT(LENGTH_MEASURE(0.01),#19864,
'DISTANCE_ACCURACY_VALUE',
'Maximum model space distance between geometric entities at asserted c
onnectivities');
#19824=UNCERTAINTY_MEASURE_WITH_UNIT(LENGTH_MEASURE(0.01),#19864,
'DISTANCE_ACCURACY_VALUE',
'Maximum model space distance between geometric entities at asserted c
onnectivities');
#19825=UNCERTAINTY_MEASURE_WITH_UNIT(LENGTH_MEASURE(0.01),#19864,
'DISTANCE_ACCURACY_VALUE',
'Maximum model space distance between geometric entities at asserted c
onnectivities');
#19826=UNCERTAINTY_MEASURE_WITH_UNIT(LENGTH_MEASURE(0.01),#19864,
'DISTANCE_ACCURACY_VALUE',
'Maximum model space distance between geometric entities at asserted c
onnectivities');
#19827=UNCERTAINTY_MEASURE_WITH_UNIT(LENGTH_MEASURE(0.01),#19864,
'DISTANCE_ACCURACY_VALUE',
'Maximum model space distance between geometric entities at asserted c
onnectivities');
#19828=UNCERTAINTY_MEASURE_WITH_UNIT(LENGTH_MEASURE(0.01),#19864,
'DISTANCE_ACCURACY_VALUE',
'Maximum model space distance between geometric entities at asserted c
onnectivities');
#19829=UNCERTAINTY_MEASURE_WITH_UNIT(LENGTH_MEASURE(0.01),#19864,
'DISTANCE_ACCURACY_VALUE',
'Maximum model space distance between geometric entities at asserted c
onnectivities');
#19830=UNCERTAINTY_MEASURE_WITH_UNIT(LENGTH_MEASURE(0.01),#19864,
'DISTANCE_ACCURACY_VALUE',
'Maximum model space distance between geometric entities at asserted c
onnectivities');
#19831=UNCERTAINTY_MEASURE_WITH_UNIT(LENGTH_MEASURE(0.01),#19864,
'DISTANCE_ACCURACY_VALUE',
'Maximum model space distance between geometric entities at asserted c
onnectivities');
#19832=UNCERTAINTY_MEASURE_WITH_UNIT(LENGTH_MEASURE(0.01),#19864,
'DISTANCE_ACCURACY_VALUE',
'Maximum model space distance between geometric entities at asserted c
onnectivities');
#19833=UNCERTAINTY_MEASURE_WITH_UNIT(LENGTH_MEASURE(0.01),#19864,
'DISTANCE_ACCURACY_VALUE',
'Maximum model space distance between geometric entities at asserted c
onnectivities');
#19834=UNCERTAINTY_MEASURE_WITH_UNIT(LENGTH_MEASURE(0.01),#19864,
'DISTANCE_ACCURACY_VALUE',
'Maximum model space distance between geometric entities at asserted c
onnectivities');
#19835=UNCERTAINTY_MEASURE_WITH_UNIT(LENGTH_MEASURE(0.01),#19864,
'DISTANCE_ACCURACY_VALUE',
'Maximum model space distance between geometric entities at asserted c
onnectivities');
#19836=UNCERTAINTY_MEASURE_WITH_UNIT(LENGTH_MEASURE(0.01),#19864,
'DISTANCE_ACCURACY_VALUE',
'Maximum model space distance between geometric entities at asserted c
onnectivities');
#19837=UNCERTAINTY_MEASURE_WITH_UNIT(LENGTH_MEASURE(0.01),#19864,
'DISTANCE_ACCURACY_VALUE',
'Maximum model space distance between geometric entities at asserted c
onnectivities');
#19838=UNCERTAINTY_MEASURE_WITH_UNIT(LENGTH_MEASURE(0.01),#19864,
'DISTANCE_ACCURACY_VALUE',
'Maximum model space distance between geometric entities at asserted c
onnectivities');
#19839=UNCERTAINTY_MEASURE_WITH_UNIT(LENGTH_MEASURE(0.01),#19864,
'DISTANCE_ACCURACY_VALUE',
'Maximum model space distance between geometric entities at asserted c
onnectivities');
#19840=UNCERTAINTY_MEASURE_WITH_UNIT(LENGTH_MEASURE(0.01),#19864,
'DISTANCE_ACCURACY_VALUE',
'Maximum model space distance between geometric entities at asserted c
onnectivities');
#19841=UNCERTAINTY_MEASURE_WITH_UNIT(LENGTH_MEASURE(0.01),#19864,
'DISTANCE_ACCURACY_VALUE',
'Maximum model space distance between geometric entities at asserted c
onnectivities');
#19842=UNCERTAINTY_MEASURE_WITH_UNIT(LENGTH_MEASURE(0.01),#19864,
'DISTANCE_ACCURACY_VALUE',
'Maximum model space distance between geometric entities at asserted c
onnectivities');
#19843=(
GEOMETRIC_REPRESENTATION_CONTEXT(3)
GLOBAL_UNCERTAINTY_ASSIGNED_CONTEXT((#19822))
GLOBAL_UNIT_ASSIGNED_CONTEXT((#19864,#19866,#19867))
REPRESENTATION_CONTEXT('','3D')
);
#19844=(
GEOMETRIC_REPRESENTATION_CONTEXT(3)
GLOBAL_UNCERTAINTY_ASSIGNED_CONTEXT((#19823))
GLOBAL_UNIT_ASSIGNED_CONTEXT((#19864,#19866,#19867))
REPRESENTATION_CONTEXT('','3D')
);
#19845=(
GEOMETRIC_REPRESENTATION_CONTEXT(3)
GLOBAL_UNCERTAINTY_ASSIGNED_CONTEXT((#19824))
GLOBAL_UNIT_ASSIGNED_CONTEXT((#19864,#19866,#19867))
REPRESENTATION_CONTEXT('','3D')
);
#19846=(
GEOMETRIC_REPRESENTATION_CONTEXT(3)
GLOBAL_UNCERTAINTY_ASSIGNED_CONTEXT((#19825))
GLOBAL_UNIT_ASSIGNED_CONTEXT((#19864,#19866,#19867))
REPRESENTATION_CONTEXT('','3D')
);
#19847=(
GEOMETRIC_REPRESENTATION_CONTEXT(3)
GLOBAL_UNCERTAINTY_ASSIGNED_CONTEXT((#19826))
GLOBAL_UNIT_ASSIGNED_CONTEXT((#19864,#19866,#19867))
REPRESENTATION_CONTEXT('','3D')
);
#19848=(
GEOMETRIC_REPRESENTATION_CONTEXT(3)
GLOBAL_UNCERTAINTY_ASSIGNED_CONTEXT((#19827))
GLOBAL_UNIT_ASSIGNED_CONTEXT((#19864,#19866,#19867))
REPRESENTATION_CONTEXT('','3D')
);
#19849=(
GEOMETRIC_REPRESENTATION_CONTEXT(3)
GLOBAL_UNCERTAINTY_ASSIGNED_CONTEXT((#19828))
GLOBAL_UNIT_ASSIGNED_CONTEXT((#19864,#19866,#19867))
REPRESENTATION_CONTEXT('','3D')
);
#19850=(
GEOMETRIC_REPRESENTATION_CONTEXT(3)
GLOBAL_UNCERTAINTY_ASSIGNED_CONTEXT((#19829))
GLOBAL_UNIT_ASSIGNED_CONTEXT((#19864,#19866,#19867))
REPRESENTATION_CONTEXT('','3D')
);
#19851=(
GEOMETRIC_REPRESENTATION_CONTEXT(3)
GLOBAL_UNCERTAINTY_ASSIGNED_CONTEXT((#19830))
GLOBAL_UNIT_ASSIGNED_CONTEXT((#19864,#19866,#19867))
REPRESENTATION_CONTEXT('','3D')
);
#19852=(
GEOMETRIC_REPRESENTATION_CONTEXT(3)
GLOBAL_UNCERTAINTY_ASSIGNED_CONTEXT((#19831))
GLOBAL_UNIT_ASSIGNED_CONTEXT((#19864,#19866,#19867))
REPRESENTATION_CONTEXT('','3D')
);
#19853=(
GEOMETRIC_REPRESENTATION_CONTEXT(3)
GLOBAL_UNCERTAINTY_ASSIGNED_CONTEXT((#19832))
GLOBAL_UNIT_ASSIGNED_CONTEXT((#19864,#19866,#19867))
REPRESENTATION_CONTEXT('','3D')
);
#19854=(
GEOMETRIC_REPRESENTATION_CONTEXT(3)
GLOBAL_UNCERTAINTY_ASSIGNED_CONTEXT((#19833))
GLOBAL_UNIT_ASSIGNED_CONTEXT((#19864,#19866,#19867))
REPRESENTATION_CONTEXT('','3D')
);
#19855=(
GEOMETRIC_REPRESENTATION_CONTEXT(3)
GLOBAL_UNCERTAINTY_ASSIGNED_CONTEXT((#19834))
GLOBAL_UNIT_ASSIGNED_CONTEXT((#19864,#19866,#19867))
REPRESENTATION_CONTEXT('','3D')
);
#19856=(
GEOMETRIC_REPRESENTATION_CONTEXT(3)
GLOBAL_UNCERTAINTY_ASSIGNED_CONTEXT((#19835))
GLOBAL_UNIT_ASSIGNED_CONTEXT((#19864,#19866,#19867))
REPRESENTATION_CONTEXT('','3D')
);
#19857=(
GEOMETRIC_REPRESENTATION_CONTEXT(3)
GLOBAL_UNCERTAINTY_ASSIGNED_CONTEXT((#19836))
GLOBAL_UNIT_ASSIGNED_CONTEXT((#19864,#19866,#19867))
REPRESENTATION_CONTEXT('','3D')
);
#19858=(
GEOMETRIC_REPRESENTATION_CONTEXT(3)
GLOBAL_UNCERTAINTY_ASSIGNED_CONTEXT((#19837))
GLOBAL_UNIT_ASSIGNED_CONTEXT((#19864,#19866,#19867))
REPRESENTATION_CONTEXT('','3D')
);
#19859=(
GEOMETRIC_REPRESENTATION_CONTEXT(3)
GLOBAL_UNCERTAINTY_ASSIGNED_CONTEXT((#19838))
GLOBAL_UNIT_ASSIGNED_CONTEXT((#19864,#19866,#19867))
REPRESENTATION_CONTEXT('','3D')
);
#19860=(
GEOMETRIC_REPRESENTATION_CONTEXT(3)
GLOBAL_UNCERTAINTY_ASSIGNED_CONTEXT((#19839))
GLOBAL_UNIT_ASSIGNED_CONTEXT((#19864,#19866,#19867))
REPRESENTATION_CONTEXT('','3D')
);
#19861=(
GEOMETRIC_REPRESENTATION_CONTEXT(3)
GLOBAL_UNCERTAINTY_ASSIGNED_CONTEXT((#19840))
GLOBAL_UNIT_ASSIGNED_CONTEXT((#19864,#19866,#19867))
REPRESENTATION_CONTEXT('','3D')
);
#19862=(
GEOMETRIC_REPRESENTATION_CONTEXT(3)
GLOBAL_UNCERTAINTY_ASSIGNED_CONTEXT((#19841))
GLOBAL_UNIT_ASSIGNED_CONTEXT((#19864,#19866,#19867))
REPRESENTATION_CONTEXT('','3D')
);
#19863=(
GEOMETRIC_REPRESENTATION_CONTEXT(3)
GLOBAL_UNCERTAINTY_ASSIGNED_CONTEXT((#19842))
GLOBAL_UNIT_ASSIGNED_CONTEXT((#19864,#19866,#19867))
REPRESENTATION_CONTEXT('','3D')
);
#19864=(
LENGTH_UNIT()
NAMED_UNIT(*)
SI_UNIT(.MILLI.,.METRE.)
);
#19865=(
LENGTH_UNIT()
NAMED_UNIT(*)
SI_UNIT($,.METRE.)
);
#19866=(
NAMED_UNIT(*)
PLANE_ANGLE_UNIT()
SI_UNIT($,.RADIAN.)
);
#19867=(
NAMED_UNIT(*)
SI_UNIT($,.STERADIAN.)
SOLID_ANGLE_UNIT()
);
#19868=SHAPE_DEFINITION_REPRESENTATION(#19888,#19934);
#19869=SHAPE_DEFINITION_REPRESENTATION(#19889,#19935);
#19870=SHAPE_DEFINITION_REPRESENTATION(#19890,#19936);
#19871=SHAPE_DEFINITION_REPRESENTATION(#19891,#19937);
#19872=SHAPE_DEFINITION_REPRESENTATION(#19892,#19938);
#19873=SHAPE_DEFINITION_REPRESENTATION(#19893,#19939);
#19874=SHAPE_DEFINITION_REPRESENTATION(#19894,#19940);
#19875=SHAPE_DEFINITION_REPRESENTATION(#19895,#19941);
#19876=SHAPE_DEFINITION_REPRESENTATION(#19896,#19942);
#19877=SHAPE_DEFINITION_REPRESENTATION(#19897,#19943);
#19878=SHAPE_DEFINITION_REPRESENTATION(#19898,#19944);
#19879=SHAPE_DEFINITION_REPRESENTATION(#19899,#19945);
#19880=SHAPE_DEFINITION_REPRESENTATION(#19900,#19946);
#19881=SHAPE_DEFINITION_REPRESENTATION(#19901,#19947);
#19882=SHAPE_DEFINITION_REPRESENTATION(#19902,#19948);
#19883=SHAPE_DEFINITION_REPRESENTATION(#19903,#19949);
#19884=SHAPE_DEFINITION_REPRESENTATION(#19904,#19950);
#19885=SHAPE_DEFINITION_REPRESENTATION(#19905,#19951);
#19886=SHAPE_DEFINITION_REPRESENTATION(#19906,#19952);
#19887=SHAPE_DEFINITION_REPRESENTATION(#19907,#19953);
#19888=PRODUCT_DEFINITION_SHAPE('',$,#19955);
#19889=PRODUCT_DEFINITION_SHAPE('',$,#19956);
#19890=PRODUCT_DEFINITION_SHAPE('',$,#19957);
#19891=PRODUCT_DEFINITION_SHAPE('',$,#19958);
#19892=PRODUCT_DEFINITION_SHAPE('',$,#19959);
#19893=PRODUCT_DEFINITION_SHAPE('',$,#19960);
#19894=PRODUCT_DEFINITION_SHAPE('',$,#19961);
#19895=PRODUCT_DEFINITION_SHAPE('',$,#19962);
#19896=PRODUCT_DEFINITION_SHAPE('',$,#19963);
#19897=PRODUCT_DEFINITION_SHAPE('',$,#19964);
#19898=PRODUCT_DEFINITION_SHAPE('',$,#19965);
#19899=PRODUCT_DEFINITION_SHAPE('',$,#19966);
#19900=PRODUCT_DEFINITION_SHAPE('',$,#19967);
#19901=PRODUCT_DEFINITION_SHAPE('',$,#19968);
#19902=PRODUCT_DEFINITION_SHAPE('',$,#19969);
#19903=PRODUCT_DEFINITION_SHAPE('',$,#19970);
#19904=PRODUCT_DEFINITION_SHAPE('',$,#19971);
#19905=PRODUCT_DEFINITION_SHAPE('',$,#19972);
#19906=PRODUCT_DEFINITION_SHAPE('',$,#19973);
#19907=PRODUCT_DEFINITION_SHAPE('',$,#19974);
#19908=PRODUCT_DEFINITION_SHAPE($,$,#89);
#19909=PRODUCT_DEFINITION_SHAPE($,$,#90);
#19910=PRODUCT_DEFINITION_SHAPE($,$,#91);
#19911=PRODUCT_DEFINITION_SHAPE($,$,#92);
#19912=PRODUCT_DEFINITION_SHAPE($,$,#93);
#19913=PRODUCT_DEFINITION_SHAPE($,$,#94);
#19914=PRODUCT_DEFINITION_SHAPE($,$,#95);
#19915=PRODUCT_DEFINITION_SHAPE($,$,#96);
#19916=PRODUCT_DEFINITION_SHAPE($,$,#97);
#19917=PRODUCT_DEFINITION_SHAPE($,$,#98);
#19918=PRODUCT_DEFINITION_SHAPE($,$,#99);
#19919=PRODUCT_DEFINITION_SHAPE($,$,#100);
#19920=PRODUCT_DEFINITION_SHAPE($,$,#101);
#19921=PRODUCT_DEFINITION_SHAPE($,$,#102);
#19922=PRODUCT_DEFINITION_SHAPE($,$,#103);
#19923=PRODUCT_DEFINITION_SHAPE($,$,#104);
#19924=PRODUCT_DEFINITION_SHAPE($,$,#105);
#19925=PRODUCT_DEFINITION_SHAPE($,$,#106);
#19926=PRODUCT_DEFINITION_SHAPE($,$,#107);
#19927=PRODUCT_DEFINITION_SHAPE($,$,#108);
#19928=PRODUCT_DEFINITION_SHAPE($,$,#109);
#19929=PRODUCT_DEFINITION_SHAPE($,$,#110);
#19930=PRODUCT_DEFINITION_SHAPE($,$,#111);
#19931=PRODUCT_DEFINITION_SHAPE($,$,#112);
#19932=PRODUCT_DEFINITION_SHAPE($,$,#113);
#19933=PRODUCT_DEFINITION_SHAPE($,$,#114);
#19934=SHAPE_REPRESENTATION('',(#6653,#7165,#7166,#7167,#7168,#7169,#7170,
#7171,#7172,#7173,#7174,#7175,#7176,#7177,#7178,#7179,#7180,#7181,#7182,
#7183,#7184,#7185,#7186,#7187,#7188,#7189,#7190),#19843);
#19935=SHAPE_REPRESENTATION('',(#6654),#19844);
#19936=SHAPE_REPRESENTATION('',(#6703),#19845);
#19937=SHAPE_REPRESENTATION('',(#6827),#19846);
#19938=SHAPE_REPRESENTATION('',(#6899),#19847);
#19939=SHAPE_REPRESENTATION('',(#6926),#19848);
#19940=SHAPE_REPRESENTATION('',(#6944),#19849);
#19941=SHAPE_REPRESENTATION('',(#6962),#19850);
#19942=SHAPE_REPRESENTATION('',(#6971),#19851);
#19943=SHAPE_REPRESENTATION('',(#6982),#19852);
#19944=SHAPE_REPRESENTATION('',(#6991),#19853);
#19945=SHAPE_REPRESENTATION('',(#7000),#19854);
#19946=SHAPE_REPRESENTATION('',(#7009),#19855);
#19947=SHAPE_REPRESENTATION('',(#7020),#19856);
#19948=SHAPE_REPRESENTATION('',(#7038),#19857);
#19949=SHAPE_REPRESENTATION('',(#7047),#19858);
#19950=SHAPE_REPRESENTATION('',(#7056),#19859);
#19951=SHAPE_REPRESENTATION('',(#7067),#19860);
#19952=SHAPE_REPRESENTATION('',(#7076),#19861);
#19953=SHAPE_REPRESENTATION('',(#7117),#19862);
#19954=PRODUCT_DEFINITION_CONTEXT('part definition',#20016,'design');
#19955=PRODUCT_DEFINITION('MAS-201','MAS-201',#19975,#19954);
#19956=PRODUCT_DEFINITION('Track channel','Track channel',#19976,#19954);
#19957=PRODUCT_DEFINITION('Guide housing','Guide housing',#19977,#19954);
#19958=PRODUCT_DEFINITION('Operating rocker','Operating rocker',#19978,
#19954);
#19959=PRODUCT_DEFINITION('Gate yoke','Gate yoke',#19979,#19954);
#19960=PRODUCT_DEFINITION('Yoke pin','Yoke pin',#19980,#19954);
#19961=PRODUCT_DEFINITION('Main pivot pin','Main pivot pin',#19981,#19954);
#19962=PRODUCT_DEFINITION('Yoke thrust washer','Yoke thrust washer',#19982,
#19954);
#19963=PRODUCT_DEFINITION('Yoke retaining ring','Yoke retaining ring',#19983,
#19954);
#19964=PRODUCT_DEFINITION('Rocker bushing','Rocker bushing',#19984,#19954);
#19965=PRODUCT_DEFINITION('Pivot thrust washer','Pivot thrust washer',#19985,
#19954);
#19966=PRODUCT_DEFINITION('Pivot spacer','Pivot spacer',#19986,#19954);
#19967=PRODUCT_DEFINITION('Pivot retaining ring','Pivot retaining ring',
#19987,#19954);
#19968=PRODUCT_DEFINITION('Travel stop pin','Travel stop pin',#19988,#19954);
#19969=PRODUCT_DEFINITION('Stop pin spacer','Stop pin spacer',#19989,#19954);
#19970=PRODUCT_DEFINITION('Stop thrust washer','Stop thrust washer',#19990,
#19954);
#19971=PRODUCT_DEFINITION('Stop retaining ring','Stop retaining ring',#19991,
#19954);
#19972=PRODUCT_DEFINITION('Handle Grip','Handle grip',#19992,#19954);
#19973=PRODUCT_DEFINITION('Shoulder screw M6x8','Shoulder screw M6x8',#19993,
#19954);
#19974=PRODUCT_DEFINITION('Socket head cap screw M4x10',
'Socket head cap screw M4x10',#19994,#19954);
#19975=PRODUCT_DEFINITION_FORMATION('',$,#20018);
#19976=PRODUCT_DEFINITION_FORMATION('',$,#20019);
#19977=PRODUCT_DEFINITION_FORMATION('',$,#20020);
#19978=PRODUCT_DEFINITION_FORMATION('',$,#20021);
#19979=PRODUCT_DEFINITION_FORMATION('',$,#20022);
#19980=PRODUCT_DEFINITION_FORMATION('',$,#20023);
#19981=PRODUCT_DEFINITION_FORMATION('',$,#20024);
#19982=PRODUCT_DEFINITION_FORMATION('',$,#20025);
#19983=PRODUCT_DEFINITION_FORMATION('',$,#20026);
#19984=PRODUCT_DEFINITION_FORMATION('',$,#20027);
#19985=PRODUCT_DEFINITION_FORMATION('',$,#20028);
#19986=PRODUCT_DEFINITION_FORMATION('',$,#20029);
#19987=PRODUCT_DEFINITION_FORMATION('',$,#20030);
#19988=PRODUCT_DEFINITION_FORMATION('',$,#20031);
#19989=PRODUCT_DEFINITION_FORMATION('',$,#20032);
#19990=PRODUCT_DEFINITION_FORMATION('',$,#20033);
#19991=PRODUCT_DEFINITION_FORMATION('',$,#20034);
#19992=PRODUCT_DEFINITION_FORMATION('',$,#20035);
#19993=PRODUCT_DEFINITION_FORMATION('',$,#20036);
#19994=PRODUCT_DEFINITION_FORMATION('',$,#20037);
#19995=PRODUCT_RELATED_PRODUCT_CATEGORY('MAS-201','MAS-201',(#20018));
#19996=PRODUCT_RELATED_PRODUCT_CATEGORY('Track channel','Track channel',
(#20019));
#19997=PRODUCT_RELATED_PRODUCT_CATEGORY('Guide housing','Guide housing',
(#20020));
#19998=PRODUCT_RELATED_PRODUCT_CATEGORY('Operating rocker',
'Operating rocker',(#20021));
#19999=PRODUCT_RELATED_PRODUCT_CATEGORY('Gate yoke','Gate yoke',(#20022));
#20000=PRODUCT_RELATED_PRODUCT_CATEGORY('Yoke pin','Yoke pin',(#20023));
#20001=PRODUCT_RELATED_PRODUCT_CATEGORY('Main pivot pin',
'Main pivot pin',(#20024));
#20002=PRODUCT_RELATED_PRODUCT_CATEGORY('Yoke thrust washer',
'Yoke thrust washer',(#20025));
#20003=PRODUCT_RELATED_PRODUCT_CATEGORY('Yoke retaining ring',
'Yoke retaining ring',(#20026));
#20004=PRODUCT_RELATED_PRODUCT_CATEGORY('Rocker bushing',
'Rocker bushing',(#20027));
#20005=PRODUCT_RELATED_PRODUCT_CATEGORY('Pivot thrust washer',
'Pivot thrust washer',(#20028));
#20006=PRODUCT_RELATED_PRODUCT_CATEGORY('Pivot spacer','Pivot spacer',(#20029));
#20007=PRODUCT_RELATED_PRODUCT_CATEGORY('Pivot retaining ring',
'Pivot retaining ring',(#20030));
#20008=PRODUCT_RELATED_PRODUCT_CATEGORY('Travel stop pin',
'Travel stop pin',(#20031));
#20009=PRODUCT_RELATED_PRODUCT_CATEGORY('Stop pin spacer',
'Stop pin spacer',(#20032));
#20010=PRODUCT_RELATED_PRODUCT_CATEGORY('Stop thrust washer',
'Stop thrust washer',(#20033));
#20011=PRODUCT_RELATED_PRODUCT_CATEGORY('Stop retaining ring',
'Stop retaining ring',(#20034));
#20012=PRODUCT_RELATED_PRODUCT_CATEGORY('Handle grip','Handle grip',(#20035));
#20013=PRODUCT_RELATED_PRODUCT_CATEGORY('Shoulder screw M6x8',
'Shoulder screw M6x8',(#20036));
#20014=PRODUCT_RELATED_PRODUCT_CATEGORY('Socket head cap screw M4x10',
'Socket head cap screw M4x10',(#20037));
#20015=APPLICATION_PROTOCOL_DEFINITION('international standard',
'automotive_design',2009,#20016);
#20016=APPLICATION_CONTEXT(
'Core Data for Automotive Mechanical Design Process');
#20017=PRODUCT_CONTEXT('part definition',#20016,'mechanical');
#20018=PRODUCT('MAS-201','MAS-201',
'Independent manual two-gate roller-track escapement for nominal30mm d
iameter20mm wide feed rollers. Opposed gates are driven by native capt
ured pin-slot loops with positive curved-slot travel stops at\X\B116de
g. Repeated gate/pin/washer/clip instances, adapted native common bear
ing families, full retaining lips and rotating polymer grip. External 
workpieces, gravity feeder/incline and mount anchors outside assembly.
 No powered-feed compatibility, impact, capacity, safety, force, wear 
or life rating.',(#20017));
#20019=PRODUCT('Track channel','Track channel',$,(#20017));
#20020=PRODUCT('Guide housing','Guide housing',$,(#20017));
#20021=PRODUCT('Operating rocker','Operating rocker',$,(#20017));
#20022=PRODUCT('Gate yoke','Gate yoke',$,(#20017));
#20023=PRODUCT('Yoke pin','Yoke pin',$,(#20017));
#20024=PRODUCT('Main pivot pin','Main pivot pin',$,(#20017));
#20025=PRODUCT('Yoke thrust washer','Yoke thrust washer',$,(#20017));
#20026=PRODUCT('Yoke retaining ring','Yoke retaining ring',$,(#20017));
#20027=PRODUCT('Rocker bushing','Rocker bushing',$,(#20017));
#20028=PRODUCT('Pivot thrust washer','Pivot thrust washer',$,(#20017));
#20029=PRODUCT('Pivot spacer','Pivot spacer',$,(#20017));
#20030=PRODUCT('Pivot retaining ring','Pivot retaining ring',$,(#20017));
#20031=PRODUCT('Travel stop pin','Travel stop pin',$,(#20017));
#20032=PRODUCT('Stop pin spacer','Stop pin spacer',$,(#20017));
#20033=PRODUCT('Stop thrust washer','Stop thrust washer',$,(#20017));
#20034=PRODUCT('Stop retaining ring','Stop retaining ring',$,(#20017));
#20035=PRODUCT('Handle Grip','Handle grip',$,(#20017));
#20036=PRODUCT('Shoulder screw M6x8','Shoulder screw M6x8',$,(#20017));
#20037=PRODUCT('Socket head cap screw M4x10',
'Socket head cap screw M4x10',$,(#20017));
#20038=PRESENTATION_STYLE_ASSIGNMENT((#20045));
#20039=PRESENTATION_STYLE_ASSIGNMENT((#20046));
#20040=PRESENTATION_STYLE_ASSIGNMENT((#20047));
#20041=PRESENTATION_STYLE_ASSIGNMENT((#20048));
#20042=PRESENTATION_STYLE_ASSIGNMENT((#20049));
#20043=PRESENTATION_STYLE_ASSIGNMENT((#20050));
#20044=PRESENTATION_STYLE_ASSIGNMENT((#20051));
#20045=SURFACE_STYLE_USAGE(.BOTH.,#20052);
#20046=SURFACE_STYLE_USAGE(.BOTH.,#20053);
#20047=SURFACE_STYLE_USAGE(.BOTH.,#20054);
#20048=SURFACE_STYLE_USAGE(.BOTH.,#20055);
#20049=SURFACE_STYLE_USAGE(.BOTH.,#20056);
#20050=SURFACE_STYLE_USAGE(.BOTH.,#20057);
#20051=SURFACE_STYLE_USAGE(.BOTH.,#20058);
#20052=SURFACE_SIDE_STYLE('',(#20059));
#20053=SURFACE_SIDE_STYLE('',(#20060));
#20054=SURFACE_SIDE_STYLE('',(#20061));
#20055=SURFACE_SIDE_STYLE('',(#20062));
#20056=SURFACE_SIDE_STYLE('',(#20063));
#20057=SURFACE_SIDE_STYLE('',(#20064));
#20058=SURFACE_SIDE_STYLE('',(#20065));
#20059=SURFACE_STYLE_FILL_AREA(#20066);
#20060=SURFACE_STYLE_FILL_AREA(#20067);
#20061=SURFACE_STYLE_FILL_AREA(#20068);
#20062=SURFACE_STYLE_FILL_AREA(#20069);
#20063=SURFACE_STYLE_FILL_AREA(#20070);
#20064=SURFACE_STYLE_FILL_AREA(#20071);
#20065=SURFACE_STYLE_FILL_AREA(#20072);
#20066=FILL_AREA_STYLE('Steel - Satin',(#20073));
#20067=FILL_AREA_STYLE('Dark blue',(#20074));
#20068=FILL_AREA_STYLE('Light blue',(#20075));
#20069=FILL_AREA_STYLE('Sky blue',(#20076));
#20070=FILL_AREA_STYLE('Gray',(#20077));
#20071=FILL_AREA_STYLE('Light gray',(#20078));
#20072=FILL_AREA_STYLE('Dark gray',(#20079));
#20073=FILL_AREA_STYLE_COLOUR('Steel - Satin',#20080);
#20074=FILL_AREA_STYLE_COLOUR('Dark blue',#20081);
#20075=FILL_AREA_STYLE_COLOUR('Light blue',#20082);
#20076=FILL_AREA_STYLE_COLOUR('Sky blue',#20083);
#20077=FILL_AREA_STYLE_COLOUR('Gray',#20084);
#20078=FILL_AREA_STYLE_COLOUR('Light gray',#20085);
#20079=FILL_AREA_STYLE_COLOUR('Dark gray',#20086);
#20080=COLOUR_RGB('Steel - Satin',0.627450980392157,0.627450980392157,0.627450980392157);
#20081=COLOUR_RGB('Dark blue',0.0901960784313725,0.270588235294118,0.513725490196078);
#20082=COLOUR_RGB('Light blue',0.662745098039216,0.831372549019608,0.949019607843137);
#20083=COLOUR_RGB('Sky blue',0.317647058823529,0.686274509803922,0.890196078431372);
#20084=COLOUR_RGB('Gray',0.407843137254902,0.447058823529412,0.498039215686275);
#20085=COLOUR_RGB('Light gray',0.725490196078431,0.752941176470588,0.792156862745098);
#20086=COLOUR_RGB('Dark gray',0.250980392156863,0.282352941176471,0.32156862745098);
ENDSEC;
END-ISO-10303-21;
